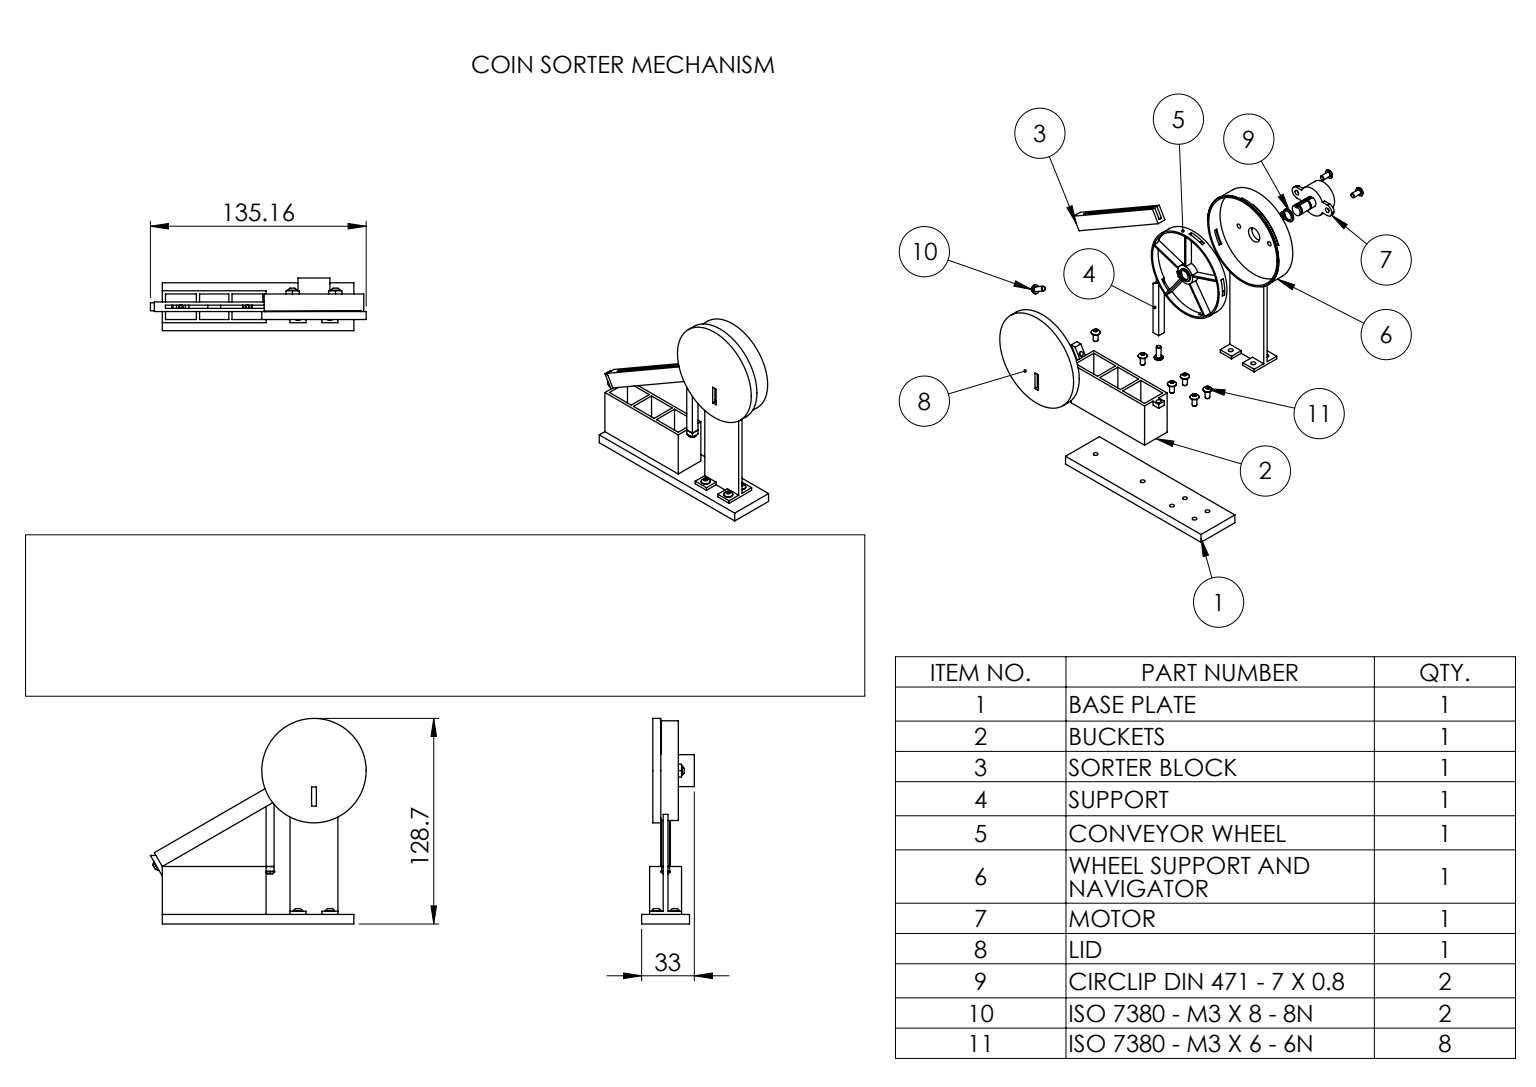
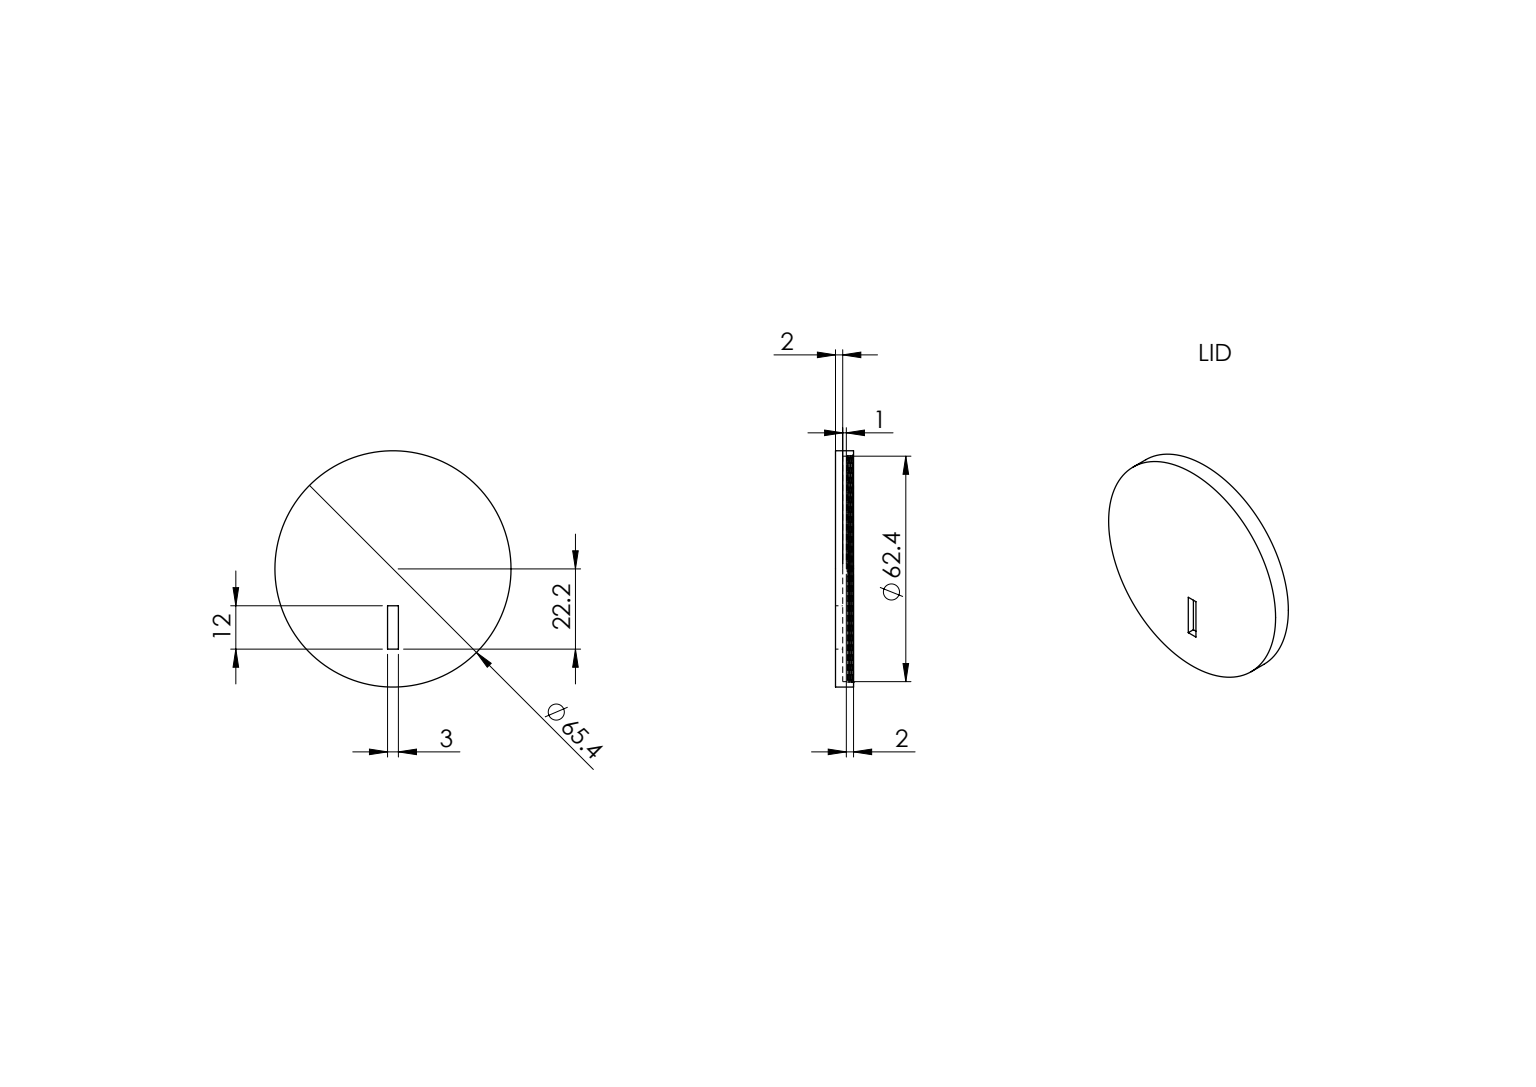
ISO-10303-21;
HEADER;
FILE_DESCRIPTION (('STEP AP214'),
    '1' );
FILE_NAME ('MAS-185',
    '2026-10-26T05:17:54',
    ( '' ),
    ( '' ),
    'SwSTEP 2.0',
    'SolidWorks 2026',
    '' );
FILE_SCHEMA (( 'AUTOMOTIVE_DESIGN' ));
ENDSEC;

DATA;
#1 = LINE ( 'NONE', #11989, #11081 ) ;
#2 = CARTESIAN_POINT ( 'NONE',  ( 35.00000000000000000, 126.3079067962035822, 4.690625000614518036 ) ) ;
#3 = ORIENTED_EDGE ( 'NONE', *, *, #1888, .T. ) ;
#4 = CARTESIAN_POINT ( 'NONE',  ( 35.00000000000000000, 126.3079067962035822, 4.296875000614517326 ) ) ;
#5 = AXIS2_PLACEMENT_3D ( 'NONE', #10923, #1108, #8837 ) ;
#6 = FACE_OUTER_BOUND ( 'NONE', #10030, .T. ) ;
#7 = ADVANCED_FACE ( 'NONE', ( #12422 ), #11435, .F. ) ;
#8 = DIRECTION ( 'NONE',  ( -0.000000000000000000, 1.000000000000000000, -0.000000000000000000 ) ) ;
#9 = CARTESIAN_POINT ( 'NONE',  ( 15.77218708916995560, 135.9950860171967975, 1.000000000000003109 ) ) ;
#10 = VECTOR ( 'NONE', #6065, 1000.000000000000000 ) ;
#11 = CARTESIAN_POINT ( 'NONE',  ( -6.666666666666660745, 2.000000000000001332, 1.599999999999986766 ) ) ;
#12 = ADVANCED_FACE ( 'NONE', ( #2550 ), #5478, .T. ) ;
#13 = CARTESIAN_POINT ( 'NONE',  ( 19.89999999999999503, 90.00000000000000000, -8.000000000000000000 ) ) ;
#14 = CARTESIAN_POINT ( 'NONE',  ( 20.00000000000000355, 121.2009999999999934, -1.499999999999999556 ) ) ;
#15 = ORIENTED_EDGE ( 'NONE', *, *, #11202, .T. ) ;
#16 = EDGE_CURVE ( 'NONE', #1898, #4275, #11568, .T. ) ;
#17 = CARTESIAN_POINT ( 'NONE',  ( 7.500000000000000000, 34.99999999999999289, -1.499999999999999556 ) ) ;
#18 = ORIENTED_EDGE ( 'NONE', *, *, #2781, .T. ) ;
#19 = EDGE_CURVE ( 'NONE', #6404, #5937, #10592, .T. ) ;
#20 = SURFACE_STYLE_FILL_AREA ( #10773 ) ;
#21 = CIRCLE ( 'NONE', #6519, 3.500000000000003109 ) ;
#22 = B_SPLINE_CURVE_WITH_KNOTS ( 'NONE', 3,
 ( #4736, #8602, #10562, #11406 ),
 .UNSPECIFIED., .F., .F.,
 ( 4, 4 ),
 ( 0.000000000000000000, 0.5999999999999992006 ),
 .UNSPECIFIED. ) ;
#23 = CARTESIAN_POINT ( 'NONE',  ( 65.00000000000000000, 90.00000000000000000, -3.000000000000000000 ) ) ;
#24 = LINE ( 'NONE', #4041, #9468 ) ;
#25 = PLANE ( 'NONE',  #12625 ) ;
#26 = ORIENTED_EDGE ( 'NONE', *, *, #8182, .F. ) ;
#27 = CARTESIAN_POINT ( 'NONE',  ( 33.50000000000000711, 79.80000000000001137, 8.000000000000000000 ) ) ;
#28 = CARTESIAN_POINT ( 'NONE',  ( 46.99999999999995737, 90.00000000000000000, -8.000000000000000000 ) ) ;
#29 = VERTEX_POINT ( 'NONE', #4640 ) ;
#30 = VECTOR ( 'NONE', #11564, 1000.000000000000114 ) ;
#31 =( NAMED_UNIT ( * ) SI_UNIT ( $, .STERADIAN. ) SOLID_ANGLE_UNIT ( ) );
#32 = CARTESIAN_POINT ( 'NONE',  ( 45.00000000000000000, 0.000000000000000000, -4.249999999999998224 ) ) ;
#33 = EDGE_LOOP ( 'NONE', ( #5496, #9068, #8693 ) ) ;
#34 = EDGE_CURVE ( 'NONE', #7938, #5032, #4885, .T. ) ;
#35 = DIRECTION ( 'NONE',  ( -0.000000000000000000, -0.000000000000000000, -1.000000000000000000 ) ) ;
#36 = VERTEX_POINT ( 'NONE', #3665 ) ;
#37 = LINE ( 'NONE', #7913, #8415 ) ;
#38 = CARTESIAN_POINT ( 'NONE',  ( 0.000000000000000000, -0.5773502691896255090, 1.000000000000000000 ) ) ;
#39 = VERTEX_POINT ( 'NONE', #7644 ) ;
#40 = COLOUR_RGB ( '',0.8941176470588234615, 0.8941176470588234615, 0.8941176470588234615 ) ;
#41 = VERTEX_POINT ( 'NONE', #12875 ) ;
#42 = FACE_BOUND ( 'NONE', #647, .T. ) ;
#43 = ORIENTED_EDGE ( 'NONE', *, *, #1360, .T. ) ;
#44 = CARTESIAN_POINT ( 'NONE',  ( 50.72178482187501203, 62.76906990284730625, 4.503125000614517148 ) ) ;
#45 = ORIENTED_EDGE ( 'NONE', *, *, #2569, .T. ) ;
#46 = DIRECTION ( 'NONE',  ( 0.000000000000000000, -0.000000000000000000, -1.000000000000000000 ) ) ;
#47 = ORIENTED_EDGE ( 'NONE', *, *, #5628, .T. ) ;
#48 = EDGE_CURVE ( 'NONE', #8414, #6329, #6123, .T. ) ;
#49 = VECTOR ( 'NONE', #8746, 1000.000000000000000 ) ;
#50 = DIRECTION ( 'NONE',  ( 0.000000000000000000, 0.000000000000000000, -1.000000000000000000 ) ) ;
#51 = CARTESIAN_POINT ( 'NONE',  ( 19.27821517812500574, 117.2309300971526937, 4.728125000614516793 ) ) ;
#52 = CARTESIAN_POINT ( 'NONE',  ( 50.59999999999999432, 117.0199925980744666, 4.850000000000000533 ) ) ;
#53 = FACE_OUTER_BOUND ( 'NONE', #7053, .T. ) ;
#54 = AXIS2_PLACEMENT_3D ( 'NONE', #9236, #4147, #9107 ) ;
#55 = APPLICATION_CONTEXT ( 'automotive_design' ) ;
#56 = PLANE ( 'NONE',  #9383 ) ;
#57 = EDGE_CURVE ( 'NONE', #11292, #8351, #9858, .T. ) ;
#59 = EDGE_CURVE ( 'NONE', #10107, #9996, #12197, .T. ) ;
#58 = VERTEX_POINT ( 'NONE', #1081 ) ;
#60 =( GEOMETRIC_REPRESENTATION_CONTEXT ( 3 ) GLOBAL_UNCERTAINTY_ASSIGNED_CONTEXT ( ( #12059 ) ) GLOBAL_UNIT_ASSIGNED_CONTEXT ( ( #6222, #10212, #383 ) ) REPRESENTATION_CONTEXT ( 'NONE', 'WORKASPACE' ) );
#61 =( BOUNDED_CURVE ( )  B_SPLINE_CURVE ( 2, ( #6392, #1163, #3141, #10390, #7315, #302, #10192 ),
 .UNSPECIFIED., .F., .F. ) 
 B_SPLINE_CURVE_WITH_KNOTS ( ( 3, 2, 2, 3 ),
 ( 0.000000000000000000, 0.03333333333333339532, 0.06666666666666679064, 0.1000000000000001860 ),
 .UNSPECIFIED. ) 
 CURVE ( )  GEOMETRIC_REPRESENTATION_ITEM ( )  RATIONAL_B_SPLINE_CURVE ( ( 1.000000000000000000, 0.8660254037844387076, 1.000000000000000000, 0.8660254037844387076, 1.000000000000000000, 0.8660254037844380415, 1.000000000000000666 ) ) 
 REPRESENTATION_ITEM ( '' )  );
#62 = CARTESIAN_POINT ( 'NONE',  ( 50.60000000000001563, 62.98000740192552627, 4.700000000000000178 ) ) ;
#63 = DIRECTION ( 'NONE',  ( 0.000000000000000000, 0.000000000000000000, 1.000000000000000000 ) ) ;
#64 = CARTESIAN_POINT ( 'NONE',  ( 42.76092309580126027, 120.3492821251987550, 2.999999999999998668 ) ) ;
#65 = ORIENTED_EDGE ( 'NONE', *, *, #9345, .T. ) ;
#66 = AXIS2_PLACEMENT_3D ( 'NONE', #9653, #8676, #680 ) ;
#67 = DIRECTION ( 'NONE',  ( 0.000000000000000000, 1.000000000000000000, 0.000000000000000000 ) ) ;
#68 = ORIENTED_EDGE ( 'NONE', *, *, #7335, .T. ) ;
#69 = CARTESIAN_POINT ( 'NONE',  ( 17.26299177799148055, 43.12143982588584379, 1.000000000000003109 ) ) ;
#70 = LINE ( 'NONE', #8139, #12259 ) ;
#71 = ORIENTED_EDGE ( 'NONE', *, *, #3443, .T. ) ;
#72 = CARTESIAN_POINT ( 'NONE',  ( -1.000000000000000000, -4.873461295629625489, -0.8000000000000000444 ) ) ;
#73 = CARTESIAN_POINT ( 'NONE',  ( 66.44356964374999563, 71.84604660189820891, 4.146875000614517859 ) ) ;
#74 = DIRECTION ( 'NONE',  ( 0.000000000000000000, 0.000000000000000000, 1.000000000000000000 ) ) ;
#75 = FACE_BOUND ( 'NONE', #11702, .T. ) ;
#76 = AXIS2_PLACEMENT_3D ( 'NONE', #9120, #143, #2199 ) ;
#77 = VECTOR ( 'NONE', #7626, 1000.000000000000000 ) ;
#78 = PLANE ( 'NONE',  #12219 ) ;
#79 = CARTESIAN_POINT ( 'NONE',  ( 9.999999999999994671, 27.00000000000000000, -2.500000000000000000 ) ) ;
#80 = FACE_BOUND ( 'NONE', #12190, .T. ) ;
#81 = EDGE_CURVE ( 'NONE', #9930, #10652, #10526, .T. ) ;
#82 = FACE_OUTER_BOUND ( 'NONE', #972, .T. ) ;
#83 = AXIS2_PLACEMENT_3D ( 'NONE', #3379, #1527, #7355 ) ;
#84 = DIRECTION ( 'NONE',  ( 2.891205793294679312E-17, 0.000000000000000000, -1.000000000000000000 ) ) ;
#85 = VERTEX_POINT ( 'NONE', #9987 ) ;
#86 = VECTOR ( 'NONE', #8647, 1000.000000000000000 ) ;
#87 = PLANE ( 'NONE',  #9136 ) ;
#88 = ORIENTED_EDGE ( 'NONE', *, *, #8982, .F. ) ;
#89 = CARTESIAN_POINT ( 'NONE',  ( -63.73205080756886076, 30.46410161513775350, 0.000000000000000000 ) ) ;
#90 = CARTESIAN_POINT ( 'NONE',  ( 3.800000000000001155, 108.0133283987163111, 4.175000001229035362 ) ) ;
#91 = AXIS2_PLACEMENT_3D ( 'NONE', #12672, #7630, #11620 ) ;
#92 = PRODUCT_DEFINITION_SHAPE ( 'NONE', 'NONE',  #12958 ) ;
#93 = DIRECTION ( 'NONE',  ( -1.000000000000000000, 0.000000000000000000, -5.337610695313252124E-17 ) ) ;
#94 = CIRCLE ( 'NONE', #5951, 0.9999999999999991118 ) ;
#95 = ORIENTED_EDGE ( 'NONE', *, *, #10637, .F. ) ;
#96 = FACE_OUTER_BOUND ( 'NONE', #3585, .T. ) ;
#97 = EDGE_CURVE ( 'NONE', #1488, #5076, #12936, .T. ) ;
#98 = CARTESIAN_POINT ( 'NONE',  ( 66.19999999999993179, 71.98667160128364628, 3.837499999999999911 ) ) ;
#99 = ORIENTED_EDGE ( 'NONE', *, *, #9615, .F. ) ;
#100 = SURFACE_SIDE_STYLE ('',( #3136 ) ) ;
#101 = CYLINDRICAL_SURFACE ( 'NONE', #2852, 1.500000000000002665 ) ;
#102 = ORIENTED_EDGE ( 'NONE', *, *, #8081, .F. ) ;
#104 = ORIENTED_EDGE ( 'NONE', *, *, #6904, .F. ) ;
#103 = CIRCLE ( 'NONE', #2000, 3.500000000000003109 ) ;
#105 = AXIS2_PLACEMENT_3D ( 'NONE', #1700, #5689, #8636 ) ;
#106 = DIRECTION ( 'NONE',  ( 0.000000000000000000, 0.000000000000000000, 1.000000000000000000 ) ) ;
#107 = DIRECTION ( 'NONE',  ( -1.000000000000000000, 0.000000000000000000, 0.000000000000000000 ) ) ;
#108 = VERTEX_POINT ( 'NONE', #7965 ) ;
#109 = EDGE_CURVE ( 'NONE', #7067, #112, #11947, .T. ) ;
#110 = ORIENTED_EDGE ( 'NONE', *, *, #11359, .T. ) ;
#111 = FACE_OUTER_BOUND ( 'NONE', #2814, .T. ) ;
#112 = VERTEX_POINT ( 'NONE', #12017 ) ;
#113 = APPLICATION_PROTOCOL_DEFINITION ( 'draft international standard', 'automotive_design', 1998, #3183 ) ;
#114 = CARTESIAN_POINT ( 'NONE',  ( 66.44356964374999563, 71.84604660189820891, 4.090625000614517504 ) ) ;
#115 = VECTOR ( 'NONE', #5469, 1000.000000000000000 ) ;
#116 = ORIENTED_EDGE ( 'NONE', *, *, #12848, .F. ) ;
#117 = CARTESIAN_POINT ( 'NONE',  ( -43.33333333333332860, 79.07477288111861924, -1.000000000000001110 ) ) ;
#118 = EDGE_LOOP ( 'NONE', ( #5135, #6023 ) ) ;
#119 = DIRECTION ( 'NONE',  ( 0.000000000000000000, 0.5000000000000000000, -0.8660254037844385966 ) ) ;
#120 = CARTESIAN_POINT ( 'NONE',  ( 19.27821517812503060, 62.76906990284727783, 3.078125000614517326 ) ) ;
#121 = DIRECTION ( 'NONE',  ( -0.8665440819333538602, -0.4991005450470686888, -4.805464830191153728E-17 ) ) ;
#122 = CARTESIAN_POINT ( 'NONE',  ( 35.00000000000000711, 53.97334320256736362, 3.425000001229034474 ) ) ;
#123 = AXIS2_PLACEMENT_3D ( 'NONE', #3186, #84, #7099 ) ;
#124 = CARTESIAN_POINT ( 'NONE',  ( 50.60000000000001563, 62.98000740192552627, 4.250000000000000000 ) ) ;
#125 = ADVANCED_FACE ( 'NONE', ( #2807 ), #25, .T. ) ;
#126 = ORIENTED_EDGE ( 'NONE', *, *, #19, .T. ) ;
#127 = CARTESIAN_POINT ( 'NONE',  ( 3.800000000000025135, 71.98667160128366049, 4.587500000000001243 ) ) ;
#128 = DIRECTION ( 'NONE',  ( 0.000000000000000000, 0.000000000000000000, -1.000000000000000000 ) ) ;
#129 = CARTESIAN_POINT ( 'NONE',  ( 59.24587011312613072, 109.7457631344924778, 2.999999999999999556 ) ) ;
#130 = ORIENTED_EDGE ( 'NONE', *, *, #2719, .F. ) ;
#131 = CARTESIAN_POINT ( 'NONE',  ( 1.040000000000000036, 0.5773502691896263972, -1.000000000000000000 ) ) ;
#132 = ORIENTED_EDGE ( 'NONE', *, *, #9753, .F. ) ;
#133 = LINE ( 'NONE', #6034, #1273 ) ;
#134 = CARTESIAN_POINT ( 'NONE',  ( 35.00000000000000000, 126.3079067962035822, 2.890625000614516882 ) ) ;
#135 = ORIENTED_EDGE ( 'NONE', *, *, #4811, .F. ) ;
#136 = EDGE_CURVE ( 'NONE', #12578, #3097, #7900, .T. ) ;
#137 = CARTESIAN_POINT ( 'NONE',  ( 66.44356964374998142, 108.1539533981018053, 3.321875000614517237 ) ) ;
#138 = DIRECTION ( 'NONE',  ( 0.000000000000000000, 0.000000000000000000, 1.000000000000000000 ) ) ;
#139 = DIRECTION ( 'NONE',  ( 0.000000000000000000, -0.000000000000000000, -1.000000000000000000 ) ) ;
#140 = CARTESIAN_POINT ( 'NONE',  ( -1.000000000000000000, -5.473461295629626022, -0.8000000000000000444 ) ) ;
#141 = ADVANCED_FACE ( 'NONE', ( #3852 ), #10839, .F. ) ;
#142 = DIRECTION ( 'NONE',  ( -0.000000000000000000, 0.000000000000000000, -1.000000000000000000 ) ) ;
#143 = DIRECTION ( 'NONE',  ( 0.8660254037844394848, 0.4999999999999985012, -0.000000000000000000 ) ) ;
#144 = DIRECTION ( 'NONE',  ( 0.000000000000000000, 0.000000000000000000, 1.000000000000000000 ) ) ;
#145 = CARTESIAN_POINT ( 'NONE',  ( 34.25000000000000000, 92.49999999999998579, 4.800000000000000711 ) ) ;
#146 = DIRECTION ( 'NONE',  ( 1.000000000000000000, 0.000000000000000000, 0.000000000000000000 ) ) ;
#147 = ORIENTED_EDGE ( 'NONE', *, *, #622, .F. ) ;
#148 = VECTOR ( 'NONE', #2125, 1000.000000000000000 ) ;
#149 = EDGE_CURVE ( 'NONE', #10256, #6226, #4830, .T. ) ;
#150 = FACE_OUTER_BOUND ( 'NONE', #10972, .T. ) ;
#151 = ORIENTED_EDGE ( 'NONE', *, *, #731, .F. ) ;
#152 =( NAMED_UNIT ( * ) SI_UNIT ( $, .STERADIAN. ) SOLID_ANGLE_UNIT ( ) );
#153 = DIRECTION ( 'NONE',  ( 1.000000000000000000, 0.000000000000000000, 0.000000000000000000 ) ) ;
#154 = CARTESIAN_POINT ( 'NONE',  ( -16.33333333333332504, 2.000000000000000000, -7.999999999999996447 ) ) ;
#155 = DIRECTION ( 'NONE',  ( -1.000000000000000000, 0.000000000000000000, -0.000000000000000000 ) ) ;
#156 = VECTOR ( 'NONE', #8810, 1000.000000000000000 ) ;
#157 = ORIENTED_EDGE ( 'NONE', *, *, #725, .T. ) ;
#158 = CARTESIAN_POINT ( 'NONE',  ( 50.00000000000000000, 2.000000000000001776, 1.500000000000001332 ) ) ;
#159 = LINE ( 'NONE', #2018, #4188 ) ;
#160 = ORIENTED_EDGE ( 'NONE', *, *, #4406, .F. ) ;
#161 = FILL_AREA_STYLE_COLOUR ( '', #4733 ) ;
#162 = ORIENTED_EDGE ( 'NONE', *, *, #11234, .F. ) ;
#163 =( LENGTH_UNIT ( ) NAMED_UNIT ( * ) SI_UNIT ( .MILLI., .METRE. ) );
#164 = ORIENTED_EDGE ( 'NONE', *, *, #8938, .T. ) ;
#165 = AXIS2_PLACEMENT_3D ( 'NONE', #5058, #1689, #12557 ) ;
#166 = LINE ( 'NONE', #6266, #6322 ) ;
#167 = CYLINDRICAL_SURFACE ( 'NONE', #2062, 31.19999999999999929 ) ;
#168 = EDGE_CURVE ( 'NONE', #9993, #9602, #10963, .T. ) ;
#169 = VERTEX_POINT ( 'NONE', #6912 ) ;
#170 = PRODUCT_DEFINITION_CONTEXT ( 'detailed design', #1838, 'design' ) ;
#171 = ORIENTED_EDGE ( 'NONE', *, *, #11272, .F. ) ;
#173 = DIRECTION ( 'NONE',  ( -0.000000000000000000, -0.000000000000000000, -1.000000000000000000 ) ) ;
#172 = AXIS2_PLACEMENT_3D ( 'NONE', #7936, #11922, #10932 ) ;
#174 = EDGE_LOOP ( 'NONE', ( #6858, #8002, #3578, #927 ) ) ;
#175 = APPLICATION_PROTOCOL_DEFINITION ( 'draft international standard', 'automotive_design', 1998, #11522 ) ;
#176 = CARTESIAN_POINT ( 'NONE',  ( 50.72178482187499071, 117.2309300971526937, 3.753125000614517592 ) ) ;
#177 = AXIS2_PLACEMENT_3D ( 'NONE', #10077, #4014, #1048 ) ;
#178 = ORIENTED_EDGE ( 'NONE', *, *, #6430, .T. ) ;
#179 = DIRECTION ( 'NONE',  ( 0.000000000000000000, 0.000000000000000000, 1.000000000000000000 ) ) ;
#180 = CARTESIAN_POINT ( 'NONE',  ( -56.80384757729341771, 34.46410161513777837, 0.000000000000000000 ) ) ;
#181 = ORIENTED_EDGE ( 'NONE', *, *, #7547, .F. ) ;
#182 = CARTESIAN_POINT ( 'NONE',  ( -60.38397459621558738, 30.66506350946110260, 0.000000000000000000 ) ) ;
#183 = CARTESIAN_POINT ( 'NONE',  ( 50.72178482187499071, 117.2309300971526937, 4.203125000614517326 ) ) ;
#184 = EDGE_CURVE ( 'NONE', #4807, #7972, #8814, .T. ) ;
#185 = DIRECTION ( 'NONE',  ( -0.3553942263724512163, 0.9347165045408831752, 0.000000000000000000 ) ) ;
#186 = AXIS2_PLACEMENT_3D ( 'NONE', #1840, #9816, #9754 ) ;
#187 = DIRECTION ( 'NONE',  ( -0.000000000000000000, -0.000000000000000000, -1.000000000000000000 ) ) ;
#188 = EDGE_CURVE ( 'NONE', #5860, #7119, #2800, .T. ) ;
#189 = ORIENTED_EDGE ( 'NONE', *, *, #6067, .T. ) ;
#190 = CARTESIAN_POINT ( 'NONE',  ( 19.40000000000000924, 117.0199925980744666, 3.125000000000000000 ) ) ;
#191 = VERTEX_POINT ( 'NONE', #1882 ) ;
#192 = LINE ( 'NONE', #5111, #8966 ) ;
#193 = VERTEX_POINT ( 'NONE', #2014 ) ;
#194 = CIRCLE ( 'NONE', #6260, 3.499999999999996003 ) ;
#195 = FACE_OUTER_BOUND ( 'NONE', #1919, .T. ) ;
#196 = ORIENTED_EDGE ( 'NONE', *, *, #12600, .T. ) ;
#197 = DIRECTION ( 'NONE',  ( -0.000000000000000000, -1.000000000000000000, -0.000000000000000000 ) ) ;
#198 = CARTESIAN_POINT ( 'NONE',  ( 3.556430356250028790, 71.84604660189818048, 3.940625000614518036 ) ) ;
#199 = EDGE_LOOP ( 'NONE', ( #6657, #5220, #2552, #8518 ) ) ;
#200 = EDGE_CURVE ( 'NONE', #11286, #1104, #9001, .T. ) ;
#201 = CARTESIAN_POINT ( 'NONE',  ( 35.00000000000000711, 53.69209320379640360, 4.071875000614516793 ) ) ;
#202 = DIRECTION ( 'NONE',  ( -0.5000000000000042188, 0.8660254037844362651, 0.000000000000000000 ) ) ;
#203 = PRODUCT_DEFINITION_SHAPE ( 'NONE', 'NONE',  #12962 ) ;
#204 = LINE ( 'NONE', #1265, #6022 ) ;
#205 = AXIS2_PLACEMENT_3D ( 'NONE', #12610, #4630, #6775 ) ;
#206 = CARTESIAN_POINT ( 'NONE',  ( 66.19999999999988916, 71.98667160128361786, 3.950000001229034829 ) ) ;
#207 = DIRECTION ( 'NONE',  ( -1.000000000000000000, 0.000000000000000000, 0.000000000000000000 ) ) ;
#208 = DIRECTION ( 'NONE',  ( -0.8660254037844365982, -0.5000000000000036637, 0.000000000000000000 ) ) ;
#209 = DIRECTION ( 'NONE',  ( 0.000000000000000000, 0.000000000000000000, 1.000000000000000000 ) ) ;
#210 = VECTOR ( 'NONE', #6420, 1000.000000000000000 ) ;
#211 = CARTESIAN_POINT ( 'NONE',  ( 1.040000000000000036, -1.154700538379251240, 1.014316938424154191E-17 ) ) ;
#212 = CARTESIAN_POINT ( 'NONE',  ( -48.33333333333332860, -5.000000000000000000, -1.500000000000003109 ) ) ;
#213 = ORIENTED_EDGE ( 'NONE', *, *, #1279, .T. ) ;
#214 = EDGE_CURVE ( 'NONE', #1472, #1154, #10317, .T. ) ;
#215 = FACE_OUTER_BOUND ( 'NONE', #2493, .T. ) ;
#216 = VERTEX_POINT ( 'NONE', #11026 ) ;
#217 = FILL_AREA_STYLE ('',( #283 ) ) ;
#218 = AXIS2_PLACEMENT_3D ( 'NONE', #4134, #11252, #317 ) ;
#219 = DIRECTION ( 'NONE',  ( 0.000000000000000000, 0.000000000000000000, -1.000000000000000000 ) ) ;
#220 = LINE ( 'NONE', #6117, #2380 ) ;
#221 = ADVANCED_FACE ( 'NONE', ( #5806 ), #2080, .F. ) ;
#222 = PLANE ( 'NONE',  #9692 ) ;
#223 = ADVANCED_FACE ( 'NONE', ( #9797 ), #3264, .F. ) ;
#224 = ORIENTED_EDGE ( 'NONE', *, *, #6026, .F. ) ;
#225 = DIRECTION ( 'NONE',  ( -0.000000000000000000, 0.000000000000000000, -1.000000000000000000 ) ) ;
#226 = DIRECTION ( 'NONE',  ( -0.000000000000000000, 1.000000000000000000, -0.000000000000000000 ) ) ;
#227 = ORIENTED_EDGE ( 'NONE', *, *, #6357, .F. ) ;
#228 =( NAMED_UNIT ( * ) SI_UNIT ( $, .STERADIAN. ) SOLID_ANGLE_UNIT ( ) );
#229 = PLANE ( 'NONE',  #10368 ) ;
#230 = ORIENTED_EDGE ( 'NONE', *, *, #426, .T. ) ;
#231 = VECTOR ( 'NONE', #9140, 1000.000000000000000 ) ;
#232 = APPLICATION_CONTEXT ( 'automotive_design' ) ;
#233 = ORIENTED_EDGE ( 'NONE', *, *, #6025, .F. ) ;
#234 = CARTESIAN_POINT ( 'NONE',  ( 2.300000000000003375, 90.00000000000000000, 3.000000000000000000 ) ) ;
#235 = DIRECTION ( 'NONE',  ( -1.000000000000000000, 0.000000000000000000, 0.000000000000000000 ) ) ;
#236 = ORIENTED_EDGE ( 'NONE', *, *, #952, .F. ) ;
#237 = VERTEX_POINT ( 'NONE', #12343 ) ;
#238 = CIRCLE ( 'NONE', #3615, 3.499999999999996003 ) ;
#239 = DIRECTION ( 'NONE',  ( 0.000000000000000000, 0.000000000000000000, -1.000000000000000000 ) ) ;
#240 = ORIENTED_EDGE ( 'NONE', *, *, #10021, .T. ) ;
#241 = CARTESIAN_POINT ( 'NONE',  ( 50.72178482187501203, 62.76906990284730625, 3.603125000614517681 ) ) ;
#242 = VERTEX_POINT ( 'NONE', #9265 ) ;
#243 = CARTESIAN_POINT ( 'NONE',  ( 4.336808689942017736E-16, 0.000000000000000000, 0.000000000000000000 ) ) ;
#244 = EDGE_CURVE ( 'NONE', #12399, #6272, #479, .T. ) ;
#245 = DIRECTION ( 'NONE',  ( -1.000000000000000000, 0.000000000000000000, -0.000000000000000000 ) ) ;
#246 = ORIENTED_EDGE ( 'NONE', *, *, #10941, .F. ) ;
#247 = DIRECTION ( 'NONE',  ( 0.000000000000000000, 0.000000000000000000, 1.000000000000000000 ) ) ;
#248 = DIRECTION ( 'NONE',  ( 1.049727191973305517E-16, 0.5150380737757253025, -0.8571673013836857979 ) ) ;
#249 = VECTOR ( 'NONE', #11495, 1000.000000000000000 ) ;
#250 = CARTESIAN_POINT ( 'NONE',  ( 50.09999999999995168, 90.00000000000000000, -10.00000000000000000 ) ) ;
#251 = FACE_OUTER_BOUND ( 'NONE', #2972, .T. ) ;
#252 = VERTEX_POINT ( 'NONE', #288 ) ;
#253 = CARTESIAN_POINT ( 'NONE',  ( 35.00000000000000711, 53.97334320256736362, 3.762500000000000178 ) ) ;
#254 = EDGE_CURVE ( 'NONE', #5137, #10011, #5741, .T. ) ;
#255 = VERTEX_POINT ( 'NONE', #12080 ) ;
#256 = DIRECTION ( 'NONE',  ( 0.000000000000000000, 0.000000000000000000, 1.000000000000000000 ) ) ;
#257 = ORIENTED_EDGE ( 'NONE', *, *, #8326, .F. ) ;
#258 =( GEOMETRIC_REPRESENTATION_CONTEXT ( 3 ) GLOBAL_UNCERTAINTY_ASSIGNED_CONTEXT ( ( #6606 ) ) GLOBAL_UNIT_ASSIGNED_CONTEXT ( ( #8219, #3259, #10305 ) ) REPRESENTATION_CONTEXT ( 'NONE', 'WORKASPACE' ) );
#259 = CYLINDRICAL_SURFACE ( 'NONE', #10517, 31.19999999999998863 ) ;
#260 = ADVANCED_FACE ( 'NONE', ( #3129 ), #3324, .T. ) ;
#261 = VERTEX_POINT ( 'NONE', #1283 ) ;
#262 = FACE_OUTER_BOUND ( 'NONE', #6852, .T. ) ;
#263 = AXIS2_PLACEMENT_3D ( 'NONE', #117, #3851, #2872 ) ;
#264 = CARTESIAN_POINT ( 'NONE',  ( 19.27821517812500574, 117.2309300971526937, 4.728125000614516793 ) ) ;
#265 = CARTESIAN_POINT ( 'NONE',  ( 3.556430356250014579, 108.1539533981018053, 3.021875000614517415 ) ) ;
#266 = LINE ( 'NONE', #12261, #1845 ) ;
#267 = CARTESIAN_POINT ( 'NONE',  ( 31.59522469073171891, 84.46307801270442894, 22.38477631085024555 ) ) ;
#268 = STYLED_ITEM ( 'NONE', ( #1181 ), #2639 ) ;
#269 = FACE_OUTER_BOUND ( 'NONE', #11895, .T. ) ;
#270 = AXIS2_PLACEMENT_3D ( 'NONE', #2486, #11695, #10523 ) ;
#271 = EDGE_CURVE ( 'NONE', #3833, #3097, #6317, .T. ) ;
#272 = CARTESIAN_POINT ( 'NONE',  ( 12.66025403784434822, 85.80682368868758658, 1.000000000000000000 ) ) ;
#273 = CARTESIAN_POINT ( 'NONE',  ( -60.00000000000000000, 23.99999999999998934, 2.500000000000000000 ) ) ;
#274 = CARTESIAN_POINT ( 'NONE',  ( 44.20597631976078645, 117.5000000000000568, 4.000000000000000000 ) ) ;
#275 = AXIS2_PLACEMENT_3D ( 'NONE', #3462, #8298, #7442 ) ;
#276 = DIRECTION ( 'NONE',  ( 1.000000000000000000, 0.000000000000000000, 0.000000000000000000 ) ) ;
#277 = CARTESIAN_POINT ( 'NONE',  ( 3.556430356250014579, 108.1539533981018053, 3.471875000614516704 ) ) ;
#278 = ORIENTED_EDGE ( 'NONE', *, *, #5223, .F. ) ;
#279 = DIRECTION ( 'NONE',  ( -0.5877852522924753575, 0.8090169943749458970, 0.000000000000000000 ) ) ;
#280 = ORIENTED_EDGE ( 'NONE', *, *, #1510, .F. ) ;
#281 = CIRCLE ( 'NONE', #7814, 4.338286831716297698 ) ;
#282 = PRODUCT ( 'lid', 'lid', '', ( #4128 ) ) ;
#283 = FILL_AREA_STYLE_COLOUR ( '', #7592 ) ;
#284 = AXIS2_PLACEMENT_3D ( 'NONE', #3967, #808, #3834 ) ;
#285 = DIRECTION ( 'NONE',  ( 0.000000000000000000, 0.000000000000000000, -1.000000000000000000 ) ) ;
#286 = FACE_OUTER_BOUND ( 'NONE', #5183, .T. ) ;
#287 = ADVANCED_FACE ( 'NONE', ( #7172 ), #1536, .F. ) ;
#288 = CARTESIAN_POINT ( 'NONE',  ( 50.09999999999995168, 90.00000000000000000, -8.000000000000000000 ) ) ;
#289 = EDGE_LOOP ( 'NONE', ( #1284, #1485, #7281, #1532 ) ) ;
#290 = AXIS2_PLACEMENT_3D ( 'NONE', #12563, #2683, #9478 ) ;
#291 = CARTESIAN_POINT ( 'NONE',  ( 35.75000000000000711, 92.49999999999998579, 4.000000000000000000 ) ) ;
#292 = CARTESIAN_POINT ( 'NONE',  ( 35.00000000000000000, 90.00000000000000000, 4.000000000000000000 ) ) ;
#293 = VECTOR ( 'NONE', #10096, 1000.000000000000000 ) ;
#294 = VERTEX_POINT ( 'NONE', #6118 ) ;
#295 =( BOUNDED_CURVE ( )  B_SPLINE_CURVE ( 2, ( #8455, #11652, #1581, #11588, #2506, #12579, #9564 ),
 .UNSPECIFIED., .F., .F. ) 
 B_SPLINE_CURVE_WITH_KNOTS ( ( 3, 2, 2, 3 ),
 ( 0.5999999999999999778, 0.6333333333333334147, 0.6666666666666667407, 0.7000000000000001776 ),
 .UNSPECIFIED. ) 
 CURVE ( )  GEOMETRIC_REPRESENTATION_ITEM ( )  RATIONAL_B_SPLINE_CURVE ( ( 1.000000000000000000, 0.8660254037844387076, 1.000000000000000000, 0.8660254037844387076, 1.000000000000000000, 0.8660254037844378194, 1.000000000000000888 ) ) 
 REPRESENTATION_ITEM ( '' )  );
#296 = CARTESIAN_POINT ( 'NONE',  ( 35.00000000000000000, 90.00000000000000000, -3.000000000000000000 ) ) ;
#297 = CARTESIAN_POINT ( 'NONE',  ( 52.49999999999996447, 94.00000000000000000, -10.00000000000000000 ) ) ;
#298 = ORIENTED_EDGE ( 'NONE', *, *, #5640, .T. ) ;
#299 = ORIENTED_EDGE ( 'NONE', *, *, #12486, .F. ) ;
#300 = EDGE_CURVE ( 'NONE', #9165, #9156, #9132, .T. ) ;
#301 = EDGE_CURVE ( 'NONE', #5352, #12120, #2388, .T. ) ;
#302 = CARTESIAN_POINT ( 'NONE',  ( 66.20000000000005969, 108.0133283987162685, 4.475000001229034297 ) ) ;
#303 = DIRECTION ( 'NONE',  ( -1.000000000000000000, 0.000000000000000000, 4.336808689942017243E-16 ) ) ;
#304 = VECTOR ( 'NONE', #4833, 1000.000000000000000 ) ;
#305 = ORIENTED_EDGE ( 'NONE', *, *, #8048, .F. ) ;
#306 = VECTOR ( 'NONE', #308, 1000.000000000000114 ) ;
#307 = VERTEX_POINT ( 'NONE', #5210 ) ;
#308 = DIRECTION ( 'NONE',  ( 0.8660254037844361541, 0.5000000000000042188, 0.000000000000000000 ) ) ;
#309 = VERTEX_POINT ( 'NONE', #6189 ) ;
#310 = EDGE_CURVE ( 'NONE', #8511, #12562, #11290, .T. ) ;
#311 = CARTESIAN_POINT ( 'NONE',  ( 50.72178482187501203, 62.76906990284730625, 4.053125000614517859 ) ) ;
#312 = ORIENTED_EDGE ( 'NONE', *, *, #4163, .F. ) ;
#313 = CIRCLE ( 'NONE', #9312, 30.19999999999999218 ) ;
#314 = LINE ( 'NONE', #2362, #12520 ) ;
#315 = ORIENTED_EDGE ( 'NONE', *, *, #7224, .T. ) ;
#316 = VECTOR ( 'NONE', #11418, 1000.000000000000000 ) ;
#317 = DIRECTION ( 'NONE',  ( 1.000000000000000000, 0.000000000000000000, 0.000000000000000000 ) ) ;
#318 = DIRECTION ( 'NONE',  ( 0.000000000000000000, 0.000000000000000000, 1.000000000000000000 ) ) ;
#319 = LINE ( 'NONE', #8516, #3101 ) ;
#320 = CONICAL_SURFACE ( 'NONE', #5556, 1732.050807568857181, 1.047197551196592746 ) ;
#321 = DIRECTION ( 'NONE',  ( -0.000000000000000000, -0.000000000000000000, -1.000000000000000000 ) ) ;
#322 = EDGE_CURVE ( 'NONE', #7840, #11587, #9067, .T. ) ;
#323 = ORIENTED_EDGE ( 'NONE', *, *, #9643, .F. ) ;
#324 =( GEOMETRIC_REPRESENTATION_CONTEXT ( 3 ) GLOBAL_UNCERTAINTY_ASSIGNED_CONTEXT ( ( #7109 ) ) GLOBAL_UNIT_ASSIGNED_CONTEXT ( ( #5148, #12551, #626 ) ) REPRESENTATION_CONTEXT ( 'NONE', 'WORKASPACE' ) );
#325 = CARTESIAN_POINT ( 'NONE',  ( 3.556430356250015024, 90.00000000000000000, 4.859375000614517326 ) ) ;
#326 = ORIENTED_EDGE ( 'NONE', *, *, #12262, .F. ) ;
#327 = CARTESIAN_POINT ( 'NONE',  ( 5.011331584521381721, 81.39071625125095011, -1.000000000000000000 ) ) ;
#328 = ORIENTED_EDGE ( 'NONE', *, *, #4950, .F. ) ;
#329 = DIRECTION ( 'NONE',  ( -0.8660254037844360431, -0.5000000000000045519, 0.000000000000000000 ) ) ;
#330 = VERTEX_POINT ( 'NONE', #11158 ) ;
#331 = LINE ( 'NONE', #11396, #210 ) ;
#332 = CARTESIAN_POINT ( 'NONE',  ( 8.335915615093540509, 106.7866562222949938, 3.000000000000001776 ) ) ;
#333 = CIRCLE ( 'NONE', #7661, 2.849999999999999201 ) ;
#334 = CARTESIAN_POINT ( 'NONE',  ( 50.72178482187499071, 117.2309300971526937, 2.909375000614517148 ) ) ;
#335 = ADVANCED_FACE ( 'NONE', ( #1345 ), #222, .F. ) ;
#336 = DIRECTION ( 'NONE',  ( 0.000000000000000000, 0.000000000000000000, 1.000000000000000000 ) ) ;
#337 = DIRECTION ( 'NONE',  ( -0.000000000000000000, -0.000000000000000000, -1.000000000000000000 ) ) ;
#338 = ADVANCED_FACE ( 'NONE', ( #7108, #5337 ), #2214, .T. ) ;
#339 = DIRECTION ( 'NONE',  ( -0.5877852522924715828, -0.8090169943749484505, 0.000000000000000000 ) ) ;
#340 = CARTESIAN_POINT ( 'NONE',  ( 66.19999999999998863, 90.00000000000000000, 4.325000000000000178 ) ) ;
#341 = DIRECTION ( 'NONE',  ( -0.3262398754384822630, 0.9452870165584014162, 0.000000000000000000 ) ) ;
#342 = VECTOR ( 'NONE', #6084, 1000.000000000000000 ) ;
#343 = LINE ( 'NONE', #3380, #2212 ) ;
#344 = CARTESIAN_POINT ( 'NONE',  ( 41.31805916882746743, 91.52713075379783447, 22.38477631085024555 ) ) ;
#345 = CARTESIAN_POINT ( 'NONE',  ( 35.00000000000000711, 53.69209320379639649, 3.621875000614517059 ) ) ;
#346 = ORIENTED_EDGE ( 'NONE', *, *, #1264, .T. ) ;
#347 = DIRECTION ( 'NONE',  ( -0.000000000000000000, 1.000000000000000000, -0.000000000000000000 ) ) ;
#348 = ORIENTED_EDGE ( 'NONE', *, *, #6229, .T. ) ;
#349 = EDGE_CURVE ( 'NONE', #2081, #11940, #2919, .T. ) ;
#350 = AXIS2_PLACEMENT_3D ( 'NONE', #7687, #12398, #1471 ) ;
#351 = ADVANCED_FACE ( 'NONE', ( #11353 ), #2405, .T. ) ;
#352 = DIRECTION ( 'NONE',  ( -1.000000000000000000, 0.000000000000000000, 0.000000000000000000 ) ) ;
#353 = CARTESIAN_POINT ( 'NONE',  ( 62.42613047537196991, 99.43702109502110886, 4.000000000000000000 ) ) ;
#354 = CARTESIAN_POINT ( 'NONE',  ( 17.55170909815984004, 66.83416404266884570, 4.000000000000000000 ) ) ;
#355 = ORIENTED_EDGE ( 'NONE', *, *, #8194, .T. ) ;
#356 = DIRECTION ( 'NONE',  ( -1.000000000000000000, 0.000000000000000000, 0.000000000000000000 ) ) ;
#357 = DIRECTION ( 'NONE',  ( -1.000000000000000000, -0.000000000000000000, -0.000000000000000000 ) ) ;
#358 = AXIS2_PLACEMENT_3D ( 'NONE', #3613, #12439, #9423 ) ;
#359 = ORIENTED_EDGE ( 'NONE', *, *, #812, .T. ) ;
#360 = DIRECTION ( 'NONE',  ( 1.000000000000000000, 0.000000000000000000, 0.000000000000000000 ) ) ;
#361 = CARTESIAN_POINT ( 'NONE',  ( 35.00000000000000000, 90.00000000000000000, -1.499999999999999556 ) ) ;
#362 = VERTEX_POINT ( 'NONE', #4108 ) ;
#363 = ORIENTED_EDGE ( 'NONE', *, *, #11341, .T. ) ;
#364 = EDGE_CURVE ( 'NONE', #1906, #5411, #4011, .T. ) ;
#365 = LINE ( 'NONE', #2416, #4028 ) ;
#366 = LINE ( 'NONE', #8567, #6016 ) ;
#367 = VECTOR ( 'NONE', #8627, 1000.000000000000114 ) ;
#368 = ORIENTED_EDGE ( 'NONE', *, *, #2982, .T. ) ;
#369 = AXIS2_PLACEMENT_3D ( 'NONE', #12355, #9278, #12488 ) ;
#370 = VERTEX_POINT ( 'NONE', #1148 ) ;
#371 = DIRECTION ( 'NONE',  ( 0.000000000000000000, 0.000000000000000000, -1.000000000000000000 ) ) ;
#372 = ORIENTED_EDGE ( 'NONE', *, *, #5978, .T. ) ;
#373 = CARTESIAN_POINT ( 'NONE',  ( 37.09602683542106405, 121.2793079999285339, 2.999999999999998668 ) ) ;
#374 = CARTESIAN_POINT ( 'NONE',  ( 66.19999999999997442, 108.0133283987163253, 4.025000001229034119 ) ) ;
#375 = ADVANCED_FACE ( 'NONE', ( #11618, #11680 ), #2535, .T. ) ;
#376 = VERTEX_POINT ( 'NONE', #8487 ) ;
#377 = CYLINDRICAL_SURFACE ( 'NONE', #4983, 1.500000000000000222 ) ;
#378 = ORIENTED_EDGE ( 'NONE', *, *, #6492, .T. ) ;
#379 = AXIS2_PLACEMENT_3D ( 'NONE', #7414, #9573, #11532 ) ;
#380 = DIRECTION ( 'NONE',  ( -1.000000000000000000, -0.000000000000000000, -0.000000000000000000 ) ) ;
#381 = FACE_BOUND ( 'NONE', #9201, .T. ) ;
#382 = CARTESIAN_POINT ( 'NONE',  ( 60.00000000000000000, -6.000000000000000000, 15.00000000000000000 ) ) ;
#383 =( NAMED_UNIT ( * ) SI_UNIT ( $, .STERADIAN. ) SOLID_ANGLE_UNIT ( ) );
#384 = AXIS2_PLACEMENT_3D ( 'NONE', #10742, #1980, #7866 ) ;
#385 = ORIENTED_EDGE ( 'NONE', *, *, #5821, .T. ) ;
#386 = DIRECTION ( 'NONE',  ( -0.000000000000000000, 1.000000000000000000, -0.000000000000000000 ) ) ;
#387 = ORIENTED_EDGE ( 'NONE', *, *, #9281, .T. ) ;
#388 = EDGE_CURVE ( 'NONE', #12930, #2334, #4689, .T. ) ;
#389 = PLANE ( 'NONE',  #10643 ) ;
#390 = EDGE_CURVE ( 'NONE', #3842, #10632, #6639, .T. ) ;
#391 = CARTESIAN_POINT ( 'NONE',  ( 50.72178482187501203, 62.76906990284730625, 4.109375000614517326 ) ) ;
#392 = ORIENTED_EDGE ( 'NONE', *, *, #8088, .T. ) ;
#393 = CIRCLE ( 'NONE', #7723, 4.000000000000003553 ) ;
#394 = CARTESIAN_POINT ( 'NONE',  ( 33.50000000000000711, 67.79999999999999716, 8.000000000000000000 ) ) ;
#395 = CARTESIAN_POINT ( 'NONE',  ( 3.591865698314129496, 91.49237114305354623, 2.999999999999999556 ) ) ;
#396 = CARTESIAN_POINT ( 'NONE',  ( 19.27821517812503060, 62.76906990284727783, 3.134375000614517237 ) ) ;
#397 = CARTESIAN_POINT ( 'NONE',  ( 0.000000000000000000, 0.000000000000000000, -0.8000000000000000444 ) ) ;
#398 = LINE ( 'NONE', #10557, #7920 ) ;
#399 = CARTESIAN_POINT ( 'NONE',  ( 38.40477530926830951, 84.46307801270444315, -1.000000000000000000 ) ) ;
#400 = AXIS2_PLACEMENT_3D ( 'NONE', #292, #2539, #8422 ) ;
#401 = CARTESIAN_POINT ( 'NONE',  ( 48.49999999999995737, 94.00000000000000000, -8.000000000000000000 ) ) ;
#402 = CARTESIAN_POINT ( 'NONE',  ( 1.750000000000000000, 0.000000000000000000, 0.000000000000000000 ) ) ;
#403 = CARTESIAN_POINT ( 'NONE',  ( 35.00000000000000000, 90.00000000000000000, 4.800000000000000711 ) ) ;
#404 = DIRECTION ( 'NONE',  ( 0.000000000000000000, 0.000000000000000000, -1.000000000000000000 ) ) ;
#405 = CARTESIAN_POINT ( 'NONE',  ( 37.99038105676688559, 21.93375672974103452, 1.000000000000000000 ) ) ;
#406 = LINE ( 'NONE', #4420, #3286 ) ;
#407 = ADVANCED_FACE ( 'NONE', ( #2595 ), #7436, .F. ) ;
#408 = VERTEX_POINT ( 'NONE', #12543 ) ;
#409 = CARTESIAN_POINT ( 'NONE',  ( 25.00000000000000000, 90.00000000000000000, -10.00000000000000000 ) ) ;
#410 = AXIS2_PLACEMENT_3D ( 'NONE', #10816, #609, #2848 ) ;
#411 = DIRECTION ( 'NONE',  ( -0.000000000000000000, 1.000000000000000000, -0.000000000000000000 ) ) ;
#412 = ORIENTED_EDGE ( 'NONE', *, *, #1216, .T. ) ;
#413 =( LENGTH_UNIT ( ) NAMED_UNIT ( * ) SI_UNIT ( .MILLI., .METRE. ) );
#414 = DIRECTION ( 'NONE',  ( 0.000000000000000000, 0.000000000000000000, -1.000000000000000000 ) ) ;
#415 = CARTESIAN_POINT ( 'NONE',  ( 50.60000000000001563, 62.98000740192552627, 4.362500001229034474 ) ) ;
#416 = CARTESIAN_POINT ( 'NONE',  ( 35.00000000000000000, 90.00000000000000000, 4.000000000000000000 ) ) ;
#417 = CIRCLE ( 'NONE', #3994, 3.499999999999996003 ) ;
#418 = ORIENTED_EDGE ( 'NONE', *, *, #1473, .F. ) ;
#419 = EDGE_CURVE ( 'NONE', #6987, #1436, #9061, .T. ) ;
#420 = FACE_OUTER_BOUND ( 'NONE', #4531, .T. ) ;
#421 = CARTESIAN_POINT ( 'NONE',  ( 0.000000000000000000, 0.5773502691896263972, -1.000000000000000000 ) ) ;
#422 = EDGE_CURVE ( 'NONE', #998, #10285, #11419, .T. ) ;
#423 = EDGE_LOOP ( 'NONE', ( #4044, #8845, #2488, #12293, #6036, #11034 ) ) ;
#424 = SHAPE_REPRESENTATION_RELATIONSHIP ( 'NONE' , 'NONE' ,  #9523, #10270 ) ;
#425 = CARTESIAN_POINT ( 'NONE',  ( -18.00412335955691745, 88.33754051161746190, 1.000000000000003109 ) ) ;
#426 = EDGE_CURVE ( 'NONE', #11653, #6806, #2729, .T. ) ;
#427 = VERTEX_POINT ( 'NONE', #1412 ) ;
#428 = CARTESIAN_POINT ( 'NONE',  ( 66.44356964374999563, 90.00000000000000000, 3.228125000614517237 ) ) ;
#429 = EDGE_LOOP ( 'NONE', ( #3770, #8264, #6534, #4530, #5902, #2222, #1505, #1439 ) ) ;
#430 = DIRECTION ( 'NONE',  ( -5.624500927088228034E-17, 1.370729058197317775E-18, 1.000000000000000000 ) ) ;
#431 = AXIS2_PLACEMENT_3D ( 'NONE', #2573, #8714, #3560 ) ;
#432 = DIRECTION ( 'NONE',  ( 0.000000000000000000, 0.000000000000000000, 1.000000000000000000 ) ) ;
#433 = ORIENTED_EDGE ( 'NONE', *, *, #4981, .F. ) ;
#434 = ORIENTED_EDGE ( 'NONE', *, *, #4950, .T. ) ;
#435 = CARTESIAN_POINT ( 'NONE',  ( 40.00000000000000000, 0.000000000000000000, 10.00000000000000000 ) ) ;
#436 = ORIENTED_EDGE ( 'NONE', *, *, #12848, .T. ) ;
#437 = CARTESIAN_POINT ( 'NONE',  ( 60.02959220194507139, 108.7322598613235414, 2.999999999999999556 ) ) ;
#438 = CONTEXT_DEPENDENT_SHAPE_REPRESENTATION ( #4763, #825 ) ;
#439 = CARTESIAN_POINT ( 'NONE',  ( 3.800000000000015365, 108.0133283987163111, 3.725000001229034297 ) ) ;
#440 = EDGE_CURVE ( 'NONE', #7916, #8087, #6573, .T. ) ;
#441 = EDGE_LOOP ( 'NONE', ( #236, #7328, #3929 ) ) ;
#442 = CIRCLE ( 'NONE', #5674, 30.00000000000000000 ) ;
#443 = VERTEX_POINT ( 'NONE', #483 ) ;
#444 = CARTESIAN_POINT ( 'NONE',  ( 35.00000000000000000, 90.00000000000000000, 4.000000000000000000 ) ) ;
#445 = ORIENTED_EDGE ( 'NONE', *, *, #1486, .T. ) ;
#446 = CARTESIAN_POINT ( 'NONE',  ( 0.000000000000000000, 2.000000000000000000, 0.000000000000000000 ) ) ;
#447 = DIRECTION ( 'NONE',  ( 0.000000000000000000, 0.000000000000000000, -1.000000000000000000 ) ) ;
#448 = VECTOR ( 'NONE', #5301, 1000.000000000000000 ) ;
#449 = ORIENTED_EDGE ( 'NONE', *, *, #16, .T. ) ;
#450 = PLANE ( 'NONE',  #6571 ) ;
#451 = VERTEX_POINT ( 'NONE', #10505 ) ;
#452 = DIRECTION ( 'NONE',  ( -0.000000000000000000, -1.000000000000000000, -0.000000000000000000 ) ) ;
#453 = EDGE_CURVE ( 'NONE', #9165, #12799, #1651, .T. ) ;
#454 = VERTEX_POINT ( 'NONE', #7693 ) ;
#455 = CARTESIAN_POINT ( 'NONE',  ( 64.54728994471078352, 100.7543353520590870, 2.858851390178780871 ) ) ;
#456 = ORIENTED_EDGE ( 'NONE', *, *, #7665, .T. ) ;
#457 = AXIS2_PLACEMENT_3D ( 'NONE', #11629, #9541, #8624 ) ;
#458 = DIRECTION ( 'NONE',  ( 0.000000000000000000, -0.000000000000000000, 1.000000000000000000 ) ) ;
#459 = DIRECTION ( 'NONE',  ( 0.000000000000000000, 0.000000000000000000, -1.000000000000000000 ) ) ;
#460 = CARTESIAN_POINT ( 'NONE',  ( 66.44356964375000985, 71.84604660189820891, 4.146875000614517859 ) ) ;
#461 = CARTESIAN_POINT ( 'NONE',  ( 40.00000000000000000, 0.000000000000000000, -10.00000000000000000 ) ) ;
#462 = EDGE_CURVE ( 'NONE', #12941, #5885, #2810, .T. ) ;
#463 = DIRECTION ( 'NONE',  ( -0.000000000000000000, -0.000000000000000000, 1.000000000000000000 ) ) ;
#464 = EDGE_CURVE ( 'NONE', #9403, #7005, #12208, .T. ) ;
#465 = DIRECTION ( 'NONE',  ( 0.000000000000000000, 0.000000000000000000, -1.000000000000000000 ) ) ;
#466 =( GEOMETRIC_REPRESENTATION_CONTEXT ( 3 ) GLOBAL_UNCERTAINTY_ASSIGNED_CONTEXT ( ( #584 ) ) GLOBAL_UNIT_ASSIGNED_CONTEXT ( ( #1408, #547, #9650 ) ) REPRESENTATION_CONTEXT ( 'NONE', 'WORKASPACE' ) );
#467 = FACE_OUTER_BOUND ( 'NONE', #11124, .T. ) ;
#468 = DIRECTION ( 'NONE',  ( 1.000000000000000000, 0.000000000000000000, 0.000000000000000000 ) ) ;
#469 = DIRECTION ( 'NONE',  ( -0.000000000000000000, 1.000000000000000000, -0.000000000000000000 ) ) ;
#470 = VECTOR ( 'NONE', #11203, 1000.000000000000000 ) ;
#471 = ADVANCED_FACE ( 'NONE', ( #3454, #10443, #9457 ), #4494, .T. ) ;
#472 = CARTESIAN_POINT ( 'NONE',  ( 35.00000000000000000, 90.00000000000000000, -8.000000000000000000 ) ) ;
#473 = CARTESIAN_POINT ( 'NONE',  ( 35.00000000000000000, 126.0266567974326222, 4.887499999999999289 ) ) ;
#474 = DIRECTION ( 'NONE',  ( -0.8660254037844360431, -0.5000000000000047740, -0.000000000000000000 ) ) ;
#475 = ORIENTED_EDGE ( 'NONE', *, *, #517, .T. ) ;
#476 = PLANE ( 'NONE',  #4013 ) ;
#477 = CARTESIAN_POINT ( 'NONE',  ( -28.99038105676692112, 50.21281292110204930, -1.000000000000000000 ) ) ;
#478 = ORIENTED_EDGE ( 'NONE', *, *, #11274, .T. ) ;
#479 = CIRCLE ( 'NONE', #1327, 28.99999999999999289 ) ;
#480 = CARTESIAN_POINT ( 'NONE',  ( 3.800000000000004707, 90.00000000000000000, 6.000000000000000000 ) ) ;
#481 = CARTESIAN_POINT ( 'NONE',  ( 8.999999999999989342, 72.14656965084313356, -1.000000000000000000 ) ) ;
#482 = ADVANCED_FACE ( 'NONE', ( #1540, #5532 ), #12604, .F. ) ;
#483 = CARTESIAN_POINT ( 'NONE',  ( 4.999999999999962697, 79.07477288111861924, 3.000000000000000000 ) ) ;
#484 = ORIENTED_EDGE ( 'NONE', *, *, #7097, .F. ) ;
#485 = VERTEX_POINT ( 'NONE', #3968 ) ;
#486 = DIRECTION ( 'NONE',  ( 4.336808689942017243E-16, 2.503857664561960972E-16, -1.000000000000000000 ) ) ;
#487 = DIRECTION ( 'NONE',  ( -0.000000000000000000, 1.000000000000000000, -0.000000000000000000 ) ) ;
#488 = VERTEX_POINT ( 'NONE', #6898 ) ;
#489 = DIRECTION ( 'NONE',  ( 0.000000000000000000, 0.000000000000000000, 1.000000000000000000 ) ) ;
#490 = AXIS2_PLACEMENT_3D ( 'NONE', #552, #3647, #7627 ) ;
#491 = CARTESIAN_POINT ( 'NONE',  ( 35.00000000000000000, 90.00000000000000000, -0.9999999999999970024 ) ) ;
#492 = ORIENTED_EDGE ( 'NONE', *, *, #5266, .F. ) ;
#493 =( GEOMETRIC_REPRESENTATION_CONTEXT ( 3 ) GLOBAL_UNCERTAINTY_ASSIGNED_CONTEXT ( ( #8293 ) ) GLOBAL_UNIT_ASSIGNED_CONTEXT ( ( #12067, #10294, #5125 ) ) REPRESENTATION_CONTEXT ( 'NONE', 'WORKASPACE' ) );
#494 = DIRECTION ( 'NONE',  ( 1.000000000000000000, 0.000000000000000000, 0.000000000000000000 ) ) ;
#495 = ORIENTED_EDGE ( 'NONE', *, *, #4508, .T. ) ;
#496 = LINE ( 'NONE', #7448, #8208 ) ;
#497 = LINE ( 'NONE', #6524, #12081 ) ;
#498 = ORIENTED_EDGE ( 'NONE', *, *, #4803, .F. ) ;
#499 = AXIS2_PLACEMENT_3D ( 'NONE', #6594, #5619, #11504 ) ;
#500 = EDGE_CURVE ( 'NONE', #6408, #3143, #4030, .T. ) ;
#501 = ORIENTED_EDGE ( 'NONE', *, *, #9357, .T. ) ;
#502 = AXIS2_PLACEMENT_3D ( 'NONE', #7934, #12717, #11921 ) ;
#503 = DIRECTION ( 'NONE',  ( -0.000000000000000000, -0.000000000000000000, -1.000000000000000000 ) ) ;
#504 = ORIENTED_EDGE ( 'NONE', *, *, #2993, .F. ) ;
#505 = CARTESIAN_POINT ( 'NONE',  ( 9.369499999999998607, 0.000000000000000000, 0.000000000000000000 ) ) ;
#506 = CONTEXT_DEPENDENT_SHAPE_REPRESENTATION ( #6758, #8984 ) ;
#507 = LINE ( 'NONE', #4515, #8154 ) ;
#508 = ORIENTED_EDGE ( 'NONE', *, *, #9196, .T. ) ;
#509 = CARTESIAN_POINT ( 'NONE',  ( -2.387319993259524598, -4.036502139894371233, 0.000000000000000000 ) ) ;
#510 = ORIENTED_EDGE ( 'NONE', *, *, #7411, .F. ) ;
#511 = CARTESIAN_POINT ( 'NONE',  ( -6.666666666666660745, 0.000000000000000000, 0.000000000000000000 ) ) ;
#513 = ORIENTED_EDGE ( 'NONE', *, *, #12102, .F. ) ;
#512 = VECTOR ( 'NONE', #6257, 1000.000000000000000 ) ;
#514 = CARTESIAN_POINT ( 'NONE',  ( 66.19999999999988916, 71.98667160128361786, 4.287500000000000533 ) ) ;
#515 = CARTESIAN_POINT ( 'NONE',  ( -3.068288344391240763, -2.655262421758692426, -0.8000000000000000444 ) ) ;
#516 = EDGE_CURVE ( 'NONE', #767, #10706, #9716, .T. ) ;
#517 = EDGE_CURVE ( 'NONE', #7067, #10542, #2603, .T. ) ;
#518 = EDGE_LOOP ( 'NONE', ( #12338, #1240, #6550, #7565 ) ) ;
#519 = CARTESIAN_POINT ( 'NONE',  ( 60.63303221600038739, 111.5086687461494392, 2.885734441893565538 ) ) ;
#520 = ORIENTED_EDGE ( 'NONE', *, *, #6993, .F. ) ;
#521 = VECTOR ( 'NONE', #8150, 1000.000000000000000 ) ;
#522 = DIRECTION ( 'NONE',  ( -0.000000000000000000, -1.000000000000000000, -0.000000000000000000 ) ) ;
#523 = VECTOR ( 'NONE', #11793, 1000.000000000000000 ) ;
#524 = ORIENTED_EDGE ( 'NONE', *, *, #12861, .T. ) ;
#525 = CARTESIAN_POINT ( 'NONE',  ( 3.556430356250015024, 90.00000000000000000, 3.959375000614517415 ) ) ;
#526 = ORIENTED_EDGE ( 'NONE', *, *, #10407, .T. ) ;
#527 = CARTESIAN_POINT ( 'NONE',  ( 3.800000000000015365, 90.00000000000000000, 4.100000000000000533 ) ) ;
#528 = CARTESIAN_POINT ( 'NONE',  ( 3.737990899702874348, 93.52352325000568101, 3.000000000000000000 ) ) ;
#529 = CARTESIAN_POINT ( 'NONE',  ( 1.040000000000000036, 0.000000000000000000, 0.000000000000000000 ) ) ;
#530 = AXIS2_PLACEMENT_3D ( 'NONE', #7357, #8344, #1205 ) ;
#531 = EDGE_CURVE ( 'NONE', #3957, #12821, #1005, .T. ) ;
#532 = CARTESIAN_POINT ( 'NONE',  ( 64.85903780527353035, 87.09520029206045422, -3.000000000000000000 ) ) ;
#533 = VECTOR ( 'NONE', #6646, 1000.000000000000000 ) ;
#534 = DIRECTION ( 'NONE',  ( 0.4999999999999987232, -0.8660254037844393737, 0.000000000000000000 ) ) ;
#535 = DIRECTION ( 'NONE',  ( -5.624500927088228034E-17, 1.370729058197317968E-18, 1.000000000000000000 ) ) ;
#536 = LINE ( 'NONE', #736, #3548 ) ;
#537 = LINE ( 'NONE', #1464, #10952 ) ;
#538 = CARTESIAN_POINT ( 'NONE',  ( 3.033375984251970081, -8.673617379884035472E-16, 0.000000000000000000 ) ) ;
#539 = EDGE_CURVE ( 'NONE', #7517, #3017, #9903, .T. ) ;
#540 = AXIS2_PLACEMENT_3D ( 'NONE', #1275, #10104, #5264 ) ;
#541 = DIRECTION ( 'NONE',  ( 0.000000000000000000, 0.000000000000000000, 1.000000000000000000 ) ) ;
#542 = CARTESIAN_POINT ( 'NONE',  ( 19.40000000000000924, 117.0199925980744666, 3.687500001229034208 ) ) ;
#543 = ORIENTED_EDGE ( 'NONE', *, *, #11638, .F. ) ;
#544 = LINE ( 'NONE', #8546, #10 ) ;
#545 = CARTESIAN_POINT ( 'NONE',  ( 1.617350269189632428, 0.000000000000000000, 0.000000000000000000 ) ) ;
#546 = ORIENTED_EDGE ( 'NONE', *, *, #10576, .T. ) ;
#547 =( NAMED_UNIT ( * ) PLANE_ANGLE_UNIT ( ) SI_UNIT ( $, .RADIAN. ) );
#548 = ADVANCED_FACE ( 'NONE', ( #11812, #12733 ), #8016, .F. ) ;
#549 = VECTOR ( 'NONE', #1621, 1000.000000000000000 ) ;
#550 = DIRECTION ( 'NONE',  ( 0.000000000000000000, -1.000000000000000000, 0.000000000000000000 ) ) ;
#551 = DIRECTION ( 'NONE',  ( -0.000000000000000000, -1.000000000000000000, -0.000000000000000000 ) ) ;
#552 = CARTESIAN_POINT ( 'NONE',  ( 35.00000000000000000, 90.00000000000000000, 6.000000000000000000 ) ) ;
#553 = ORIENTED_EDGE ( 'NONE', *, *, #4093, .T. ) ;
#554 = DIRECTION ( 'NONE',  ( 0.000000000000000000, 0.000000000000000000, 1.000000000000000000 ) ) ;
#555 = CARTESIAN_POINT ( 'NONE',  ( 0.1038759689922479496, -3.348389132562988646, -0.8000000000000000444 ) ) ;
#556 = ADVANCED_FACE ( 'NONE', ( #3049, #10826 ), #5003, .F. ) ;
#557 = ORIENTED_EDGE ( 'NONE', *, *, #7447, .F. ) ;
#558 = CARTESIAN_POINT ( 'NONE',  ( 35.00000000000000000, 90.00000000000000000, 4.000000000000000000 ) ) ;
#559 = DIRECTION ( 'NONE',  ( 1.000000000000000000, -0.000000000000000000, 0.000000000000000000 ) ) ;
#560 = ORIENTED_EDGE ( 'NONE', *, *, #12372, .T. ) ;
#561 = VECTOR ( 'NONE', #4344, 999.9999999999998863 ) ;
#562 = FACE_OUTER_BOUND ( 'NONE', #1188, .T. ) ;
#563 = ORIENTED_EDGE ( 'NONE', *, *, #5905, .F. ) ;
#564 = CARTESIAN_POINT ( 'NONE',  ( 45.39999948872177526, 60.58435772187547030, 3.000000000000000000 ) ) ;
#565 = FACE_OUTER_BOUND ( 'NONE', #1775, .T. ) ;
#566 = ORIENTED_EDGE ( 'NONE', *, *, #10069, .F. ) ;
#567 = FACE_OUTER_BOUND ( 'NONE', #6153, .T. ) ;
#568 = ORIENTED_EDGE ( 'NONE', *, *, #10862, .T. ) ;
#569 = AXIS2_PLACEMENT_3D ( 'NONE', #2591, #4682, #2724 ) ;
#570 = CARTESIAN_POINT ( 'NONE',  ( 8.499999999999998224, 79.07477288111861924, 1.000000000000000000 ) ) ;
#571 = VERTEX_POINT ( 'NONE', #2859 ) ;
#572 = DIRECTION ( 'NONE',  ( -1.000000000000000000, 0.000000000000000000, 0.000000000000000000 ) ) ;
#573 = SHAPE_DEFINITION_REPRESENTATION ( #2509, #985 ) ;
#574 = CARTESIAN_POINT ( 'NONE',  ( 3.800000000000015365, 90.00000000000000000, 3.200000000000000178 ) ) ;
#575 = ORIENTED_EDGE ( 'NONE', *, *, #4120, .F. ) ;
#576 = ORIENTED_EDGE ( 'NONE', *, *, #12211, .T. ) ;
#577 = SURFACE_STYLE_FILL_AREA ( #1504 ) ;
#578 = ORIENTED_EDGE ( 'NONE', *, *, #7988, .T. ) ;
#579 = ADVANCED_FACE ( 'NONE', ( #1999 ), #8988, .F. ) ;
#580 = VECTOR ( 'NONE', #12744, 1000.000000000000000 ) ;
#581 = AXIS2_PLACEMENT_3D ( 'NONE', #6283, #2043, #10989 ) ;
#582 = CARTESIAN_POINT ( 'NONE',  ( 35.39078165856646763, 58.73470357045291479, 3.000000000000001332 ) ) ;
#583 = DIRECTION ( 'NONE',  ( -1.000000000000000000, 0.000000000000000000, 0.000000000000000000 ) ) ;
#584 = UNCERTAINTY_MEASURE_WITH_UNIT (LENGTH_MEASURE( 1.000000000000000082E-05 ), #1408, 'distance_accuracy_value', 'NONE');
#585 = VERTEX_POINT ( 'NONE', #1932 ) ;
#586 = CARTESIAN_POINT ( 'NONE',  ( 35.00000000000000711, 53.69209320379640360, 3.621875000614517059 ) ) ;
#587 = VERTEX_POINT ( 'NONE', #749 ) ;
#588 = PLANE ( 'NONE',  #11054 ) ;
#589 = VECTOR ( 'NONE', #11996, 1000.000000000000000 ) ;
#590 = ORIENTED_EDGE ( 'NONE', *, *, #5677, .T. ) ;
#591 = CARTESIAN_POINT ( 'NONE',  ( 3.556430356250015024, 90.00000000000000000, 3.509375000614517681 ) ) ;
#592 = ORIENTED_EDGE ( 'NONE', *, *, #5905, .T. ) ;
#593 = ADVANCED_FACE ( 'NONE', ( #5912, #5791 ), #3774, .T. ) ;
#594 = CARTESIAN_POINT ( 'NONE',  ( 66.20000000000004547, 108.0133283987162969, 3.912500000000000977 ) ) ;
#595 = DIRECTION ( 'NONE',  ( -0.000000000000000000, -1.000000000000000000, -0.000000000000000000 ) ) ;
#596 = EDGE_CURVE ( 'NONE', #330, #4076, #4069, .T. ) ;
#597 = DIRECTION ( 'NONE',  ( -0.000000000000000000, -1.000000000000000000, -0.000000000000000000 ) ) ;
#598 = CARTESIAN_POINT ( 'NONE',  ( 0.000000000000000000, -0.5773502691896256200, -1.000000000000000000 ) ) ;
#600 = AXIS2_PLACEMENT_3D ( 'NONE', #4155, #337, #1325 ) ;
#599 = DIRECTION ( 'NONE',  ( 1.000000000000000000, 0.000000000000000000, 0.000000000000000000 ) ) ;
#601 = DIRECTION ( 'NONE',  ( -0.000000000000000000, 1.000000000000000000, -0.000000000000000000 ) ) ;
#602 = CARTESIAN_POINT ( 'NONE',  ( 35.00000000000000000, 90.00000000000000000, -0.9999999999999970024 ) ) ;
#603 = DIRECTION ( 'NONE',  ( 0.000000000000000000, 0.5150380737757253025, 0.8571673013836857979 ) ) ;
#604 = CARTESIAN_POINT ( 'NONE',  ( -6.666666666666660745, 2.000000000000001332, -1.599999999999986766 ) ) ;
#605 = VECTOR ( 'NONE', #12118, 1000.000000000000000 ) ;
#606 = FACE_OUTER_BOUND ( 'NONE', #6514, .T. ) ;
#607 = ADVANCED_FACE ( 'NONE', ( #809 ), #12923, .T. ) ;
#608 = VECTOR ( 'NONE', #6526, 1000.000000000000000 ) ;
#609 = DIRECTION ( 'NONE',  ( -1.000000000000000000, -0.000000000000000000, -0.000000000000000000 ) ) ;
#610 = CARTESIAN_POINT ( 'NONE',  ( 35.00000000000000000, 90.00000000000000000, -1.000000000000000000 ) ) ;
#611 = ORIENTED_EDGE ( 'NONE', *, *, #2370, .T. ) ;
#612 = CARTESIAN_POINT ( 'NONE',  ( 50.59999999999999432, 117.0199925980744666, 4.400000000000000355 ) ) ;
#613 = LINE ( 'NONE', #545, #2256 ) ;
#614 = ORIENTED_EDGE ( 'NONE', *, *, #6666, .F. ) ;
#615 =( NAMED_UNIT ( * ) SI_UNIT ( $, .STERADIAN. ) SOLID_ANGLE_UNIT ( ) );
#616 = VECTOR ( 'NONE', #1823, 1000.000000000000000 ) ;
#617 = DIRECTION ( 'NONE',  ( 1.000000000000000000, 0.000000000000000000, 0.000000000000000000 ) ) ;
#618 = CARTESIAN_POINT ( 'NONE',  ( 48.11036777325283964, 61.54261756562988239, 3.006515308376277229 ) ) ;
#619 = VERTEX_POINT ( 'NONE', #8800 ) ;
#620 = PLANE ( 'NONE',  #2626 ) ;
#621 = CARTESIAN_POINT ( 'NONE',  ( 19.27821517812503060, 62.76906990284727783, 4.428125000614516971 ) ) ;
#622 = EDGE_CURVE ( 'NONE', #3150, #9073, #1826, .T. ) ;
#623 = ORIENTED_EDGE ( 'NONE', *, *, #10337, .T. ) ;
#624 = AXIS2_PLACEMENT_3D ( 'NONE', #12004, #1206, #5133 ) ;
#625 = DIRECTION ( 'NONE',  ( -0.8746197064978278313, 0.4848096214037562746, 1.049727191973305270E-16 ) ) ;
#626 =( NAMED_UNIT ( * ) SI_UNIT ( $, .STERADIAN. ) SOLID_ANGLE_UNIT ( ) );
#627 = ORIENTED_EDGE ( 'NONE', *, *, #322, .T. ) ;
#628 = LINE ( 'NONE', #4760, #11001 ) ;
#629 = ORIENTED_EDGE ( 'NONE', *, *, #7794, .T. ) ;
#630 = CARTESIAN_POINT ( 'NONE',  ( 18.35873618070580093, 66.24461453698026503, 4.000000000000000000 ) ) ;
#631 = CYLINDRICAL_SURFACE ( 'NONE', #12303, 0.9999999999999991118 ) ;
#632 = EDGE_CURVE ( 'NONE', #11636, #4911, #11998, .T. ) ;
#633 = ADVANCED_FACE ( 'NONE', ( #3905 ), #2920, .F. ) ;
#634 = CIRCLE ( 'NONE', #12768, 3.350000000000000089 ) ;
#635 = DIRECTION ( 'NONE',  ( -1.000000000000000000, 0.000000000000000000, 0.000000000000000000 ) ) ;
#636 = CARTESIAN_POINT ( 'NONE',  ( 35.75000000000000711, 92.49999999999998579, -3.000000000000000000 ) ) ;
#637 = DIRECTION ( 'NONE',  ( 0.000000000000000000, 0.000000000000000000, -1.000000000000000000 ) ) ;
#638 = ORIENTED_EDGE ( 'NONE', *, *, #97, .F. ) ;
#639 = DIRECTION ( 'NONE',  ( -1.000000000000000000, -0.000000000000000000, -0.000000000000000000 ) ) ;
#640 = CONTEXT_DEPENDENT_SHAPE_REPRESENTATION ( #11014, #5527 ) ;
#641 = CARTESIAN_POINT ( 'NONE',  ( 19.40000000000002700, 62.98000740192551206, 3.837500001229034563 ) ) ;
#642 = ORIENTED_EDGE ( 'NONE', *, *, #5141, .F. ) ;
#643 = SURFACE_STYLE_USAGE ( .BOTH. , #9675 ) ;
#644 = ORIENTED_EDGE ( 'NONE', *, *, #5801, .F. ) ;
#645 = VECTOR ( 'NONE', #10208, 1000.000000000000227 ) ;
#646 = DIRECTION ( 'NONE',  ( 0.000000000000000000, 0.000000000000000000, 1.000000000000000000 ) ) ;
#647 = EDGE_LOOP ( 'NONE', ( #10608, #8614 ) ) ;
#648 = CARTESIAN_POINT ( 'NONE',  ( 15.29066239423023887, 65.64213830996915533, 3.000000000000000444 ) ) ;
#649 = LINE ( 'NONE', #2821, #9778 ) ;
#650 = ORIENTED_EDGE ( 'NONE', *, *, #2075, .F. ) ;
#651 = CARTESIAN_POINT ( 'NONE',  ( 64.54728993811707483, 100.7543353701752125, 2.858851390224067313 ) ) ;
#652 = EDGE_LOOP ( 'NONE', ( #3973, #10053 ) ) ;
#653 = EDGE_CURVE ( 'NONE', #6728, #2032, #6175, .T. ) ;
#654 = CARTESIAN_POINT ( 'NONE',  ( -60.00000000000000000, 30.00000000000000000, 2.500000000000000000 ) ) ;
#655 = VERTEX_POINT ( 'NONE', #9185 ) ;
#656 = CARTESIAN_POINT ( 'NONE',  ( 50.72178482187501203, 62.76906990284730625, 3.209375000614517415 ) ) ;
#657 = ORIENTED_EDGE ( 'NONE', *, *, #9994, .T. ) ;
#658 = DIRECTION ( 'NONE',  ( 0.000000000000000000, -1.000000000000000000, 0.000000000000000000 ) ) ;
#659 = CARTESIAN_POINT ( 'NONE',  ( 6.499999999999999112, 68.39379290111055809, 2.999999999999960032 ) ) ;
#660 = FACE_OUTER_BOUND ( 'NONE', #1254, .T. ) ;
#661 = AXIS2_PLACEMENT_3D ( 'NONE', #10121, #1470, #8480 ) ;
#662 = CARTESIAN_POINT ( 'NONE',  ( 19.27821517812500574, 117.2309300971526937, 4.728125000614516793 ) ) ;
#663 = EDGE_CURVE ( 'NONE', #698, #11775, #6107, .T. ) ;
#664 = DIRECTION ( 'NONE',  ( -0.000000000000000000, -0.000000000000000000, -1.000000000000000000 ) ) ;
#665 = CARTESIAN_POINT ( 'NONE',  ( 35.00000000000000000, 90.00000000000000000, 4.000000000000000000 ) ) ;
#666 = EDGE_CURVE ( 'NONE', #8482, #12120, #12330, .T. ) ;
#667 = CARTESIAN_POINT ( 'NONE',  ( -54.07179676972453564, 35.73205080756890339, -1.000000000000000000 ) ) ;
#668 = DIRECTION ( 'NONE',  ( 0.000000000000000000, 1.000000000000000000, -1.370729058197317775E-18 ) ) ;
#669 = VECTOR ( 'NONE', #1046, 1000.000000000000000 ) ;
#670 = PLANE ( 'NONE',  #6171 ) ;
#671 = DIRECTION ( 'NONE',  ( 0.8660254037844361541, 0.5000000000000042188, 0.000000000000000000 ) ) ;
#672 = CARTESIAN_POINT ( 'NONE',  ( 66.44356964374998142, 108.1539533981018053, 3.771875000614516971 ) ) ;
#673 = ORIENTED_EDGE ( 'NONE', *, *, #3401, .T. ) ;
#674 = DIRECTION ( 'NONE',  ( -0.000000000000000000, 1.000000000000000000, -0.000000000000000000 ) ) ;
#675 = DIRECTION ( 'NONE',  ( 5.624500927088228034E-17, -1.370729058197317775E-18, -1.000000000000000000 ) ) ;
#676 = ORIENTED_EDGE ( 'NONE', *, *, #11289, .T. ) ;
#677 = VECTOR ( 'NONE', #9665, 1000.000000000000000 ) ;
#678 = EDGE_CURVE ( 'NONE', #12162, #3526, #8342, .T. ) ;
#679 = DIRECTION ( 'NONE',  ( 0.9510565162951554186, -0.3090169943749414005, 0.000000000000000000 ) ) ;
#680 = DIRECTION ( 'NONE',  ( 1.000000000000000000, 0.000000000000000000, -0.000000000000000000 ) ) ;
#681 = VERTEX_POINT ( 'NONE', #7030 ) ;
#682 = CARTESIAN_POINT ( 'NONE',  ( 7.500000000000000000, 30.00000000000000000, 0.000000000000000000 ) ) ;
#683 = CARTESIAN_POINT ( 'NONE',  ( 66.44356964374998142, 108.1539533981018053, 3.715625000614517948 ) ) ;
#684 = COLOUR_RGB ( '',0.8941176470588234615, 0.8941176470588234615, 0.8941176470588234615 ) ;
#685 = DIRECTION ( 'NONE',  ( -0.8660254037844361541, -0.5000000000000042188, 9.389466242107218061E-17 ) ) ;
#686 = DIRECTION ( 'NONE',  ( 0.000000000000000000, 0.000000000000000000, 1.000000000000000000 ) ) ;
#687 = ORIENTED_EDGE ( 'NONE', *, *, #453, .F. ) ;
#688 = CARTESIAN_POINT ( 'NONE',  ( 7.500000000000000000, 27.00000000000000000, 0.000000000000000000 ) ) ;
#689 = ORIENTED_EDGE ( 'NONE', *, *, #1063, .F. ) ;
#690 = VECTOR ( 'NONE', #8750, 1000.000000000000114 ) ;
#691 = CARTESIAN_POINT ( 'NONE',  ( 25.00000000000000355, 0.000000000000000000, 4.249999999999998224 ) ) ;
#692 = LINE ( 'NONE', #4702, #11877 ) ;
#693 = EDGE_CURVE ( 'NONE', #12083, #4963, #12636, .T. ) ;
#694 = PRESENTATION_LAYER_ASSIGNMENT (  '', '', ( #11566 ) ) ;
#695 = LINE ( 'NONE', #11320, #4590 ) ;
#696 = ORIENTED_EDGE ( 'NONE', *, *, #6826, .F. ) ;
#697 = CARTESIAN_POINT ( 'NONE',  ( 0.000000000000000000, 2.000000000000000000, 0.000000000000000000 ) ) ;
#698 = VERTEX_POINT ( 'NONE', #11012 ) ;
#699 = CLOSED_SHELL ( 'NONE', ( #4681, #2294, #5712, #12137, #6395, #6284, #10454, #6271, #7033, #8769, #9664, #6996, #3078, #6506, #5758, #9872, #10478, #5588, #2469, #1397, #4829, #5175, #6473, #11028, #2843, #8926, #11939, #3918, #407, #9755, #9220, #11801, #9117, #7996, #2544, #5940, #1715, #12395, #866, #5366, #1669, #7054, #12542, #2318, #6182, #10197, #10507 ) ) ;
#700 = DIRECTION ( 'NONE',  ( 0.000000000000000000, 1.000000000000000000, 0.000000000000000000 ) ) ;
#701 = CONTEXT_DEPENDENT_SHAPE_REPRESENTATION ( #4097, #203 ) ;
#702 = CARTESIAN_POINT ( 'NONE',  ( 0.000000000000000000, 0.000000000000000000, 1.499999999999999556 ) ) ;
#703 = VERTEX_POINT ( 'NONE', #4159 ) ;
#704 = CARTESIAN_POINT ( 'NONE',  ( 35.00000000000000000, 90.00000000000000000, -10.00000000000000000 ) ) ;
#705 = EDGE_CURVE ( 'NONE', #12083, #370, #10296, .T. ) ;
#706 = ORIENTED_EDGE ( 'NONE', *, *, #3432, .T. ) ;
#707 = EDGE_CURVE ( 'NONE', #1672, #10599, #4291, .T. ) ;
#708 = PRODUCT_DEFINITION_FORMATION_WITH_SPECIFIED_SOURCE ( 'ANY', '', #2726, .NOT_KNOWN. ) ;
#709 = LINE ( 'NONE', #2754, #11300 ) ;
#710 = ORIENTED_EDGE ( 'NONE', *, *, #10661, .T. ) ;
#711 = DIRECTION ( 'NONE',  ( 0.000000000000000000, 0.5150380737757253025, 0.8571673013836857979 ) ) ;
#712 = LINE ( 'NONE', #12759, #4156 ) ;
#713 = AXIS2_PLACEMENT_3D ( 'NONE', #1399, #12460, #4544 ) ;
#714 = AXIS2_PLACEMENT_3D ( 'NONE', #11287, #12341, #11156 ) ;
#715 = ADVANCED_FACE ( 'NONE', ( #10234 ), #11079, .T. ) ;
#716 = VERTEX_POINT ( 'NONE', #3314 ) ;
#717 = DIRECTION ( 'NONE',  ( 0.000000000000000000, 0.000000000000000000, 1.000000000000000000 ) ) ;
#718 = VERTEX_POINT ( 'NONE', #4225 ) ;
#719 = FACE_OUTER_BOUND ( 'NONE', #6790, .T. ) ;
#720 = EDGE_LOOP ( 'NONE', ( #4308, #11552, #5164, #9758 ) ) ;
#721 = CIRCLE ( 'NONE', #499, 10.00000000000000178 ) ;
#722 = CARTESIAN_POINT ( 'NONE',  ( 3.556430356250014579, 108.1539533981018053, 3.865625000614517415 ) ) ;
#723 = PRODUCT_DEFINITION_SHAPE ( 'NONE', 'NONE',  #12956 ) ;
#724 = ORIENTED_EDGE ( 'NONE', *, *, #4951, .F. ) ;
#725 = EDGE_CURVE ( 'NONE', #12624, #3688, #9320, .T. ) ;
#726 = AXIS2_PLACEMENT_3D ( 'NONE', #602, #12590, #3632 ) ;
#727 = CARTESIAN_POINT ( 'NONE',  ( -60.00000000000000000, 30.00000000000000000, 9.999999999999996447 ) ) ;
#728 = DIRECTION ( 'NONE',  ( 0.000000000000000000, -1.000000000000000000, 0.000000000000000000 ) ) ;
#729 = FILL_AREA_STYLE_COLOUR ( '', #2356 ) ;
#730 = CARTESIAN_POINT ( 'NONE',  ( 66.19999999999998863, 90.00000000000000000, 4.437500001229033764 ) ) ;
#731 = EDGE_CURVE ( 'NONE', #10645, #11257, #10099, .T. ) ;
#732 = CIRCLE ( 'NONE', #5327, 1.499999999999999556 ) ;
#733 = CARTESIAN_POINT ( 'NONE',  ( -61.00000000000000711, 26.13129029178200469, 0.9999999999999926725 ) ) ;
#734 = CIRCLE ( 'NONE', #6785, 1.599999999999997202 ) ;
#735 = CARTESIAN_POINT ( 'NONE',  ( 66.19999999999997442, 108.0133283987163253, 4.812500000000000000 ) ) ;
#736 = CARTESIAN_POINT ( 'NONE',  ( 35.75000000000000711, 92.49999999999998579, -4.802775637732004554 ) ) ;
#737 = DIRECTION ( 'NONE',  ( -0.000000000000000000, -0.000000000000000000, -1.000000000000000000 ) ) ;
#738 = CARTESIAN_POINT ( 'NONE',  ( 31.50000000000000000, 90.00000000000000000, -8.000000000000000000 ) ) ;
#739 = EDGE_CURVE ( 'NONE', #5916, #6728, #5927, .T. ) ;
#740 = CARTESIAN_POINT ( 'NONE',  ( 1.617350269189632428, 0.000000000000000000, 0.000000000000000000 ) ) ;
#741 = CARTESIAN_POINT ( 'NONE',  ( 19.27821517812500574, 117.2309300971526937, 3.884375000614516793 ) ) ;
#742 = ORIENTED_EDGE ( 'NONE', *, *, #6361, .T. ) ;
#743 = CIRCLE ( 'NONE', #2637, 1.500000000000001332 ) ;
#744 = CARTESIAN_POINT ( 'NONE',  ( 66.20000000000000284, 71.98667160128370313, 4.287500000000000533 ) ) ;
#745 = DIRECTION ( 'NONE',  ( 1.000000000000000000, 1.281026566875180806E-14, 0.000000000000000000 ) ) ;
#746 = ORIENTED_EDGE ( 'NONE', *, *, #952, .T. ) ;
#747 = EDGE_CURVE ( 'NONE', #10649, #11707, #5061, .T. ) ;
#748 = DIRECTION ( 'NONE',  ( 0.000000000000000000, 0.000000000000000000, -1.000000000000000000 ) ) ;
#749 = CARTESIAN_POINT ( 'NONE',  ( 5.000000000000007994, 90.00000000000000000, -3.000000000000000000 ) ) ;
#750 = VECTOR ( 'NONE', #11166, 1000.000000000000000 ) ;
#751 = CARTESIAN_POINT ( 'NONE',  ( 5.000000000000004441, 30.00000000000000000, -2.500000000000000444 ) ) ;
#752 = CARTESIAN_POINT ( 'NONE',  ( 3.556430356250014579, 108.1539533981018053, 3.415625000614516793 ) ) ;
#753 = DIRECTION ( 'NONE',  ( 1.000000000000000000, 0.000000000000000000, 0.000000000000000000 ) ) ;
#754 = CARTESIAN_POINT ( 'NONE',  ( 3.556430356250015024, 90.00000000000000000, 4.859375000614517326 ) ) ;
#755 = EDGE_LOOP ( 'NONE', ( #10469, #5474, #7145, #11199 ) ) ;
#756 = EDGE_CURVE ( 'NONE', #5282, #3511, #6243, .T. ) ;
#757 = CARTESIAN_POINT ( 'NONE',  ( 3.800000000000001155, 108.0133283987163111, 4.512500000000001066 ) ) ;
#758 = ORIENTED_EDGE ( 'NONE', *, *, #6666, .T. ) ;
#759 = ADVANCED_FACE ( 'NONE', ( #3115 ), #7095, .F. ) ;
#760 = CIRCLE ( 'NONE', #2246, 1.500000000000001332 ) ;
#761 =( LENGTH_UNIT ( ) NAMED_UNIT ( * ) SI_UNIT ( .MILLI., .METRE. ) );
#762 = DIRECTION ( 'NONE',  ( -0.000000000000000000, -1.000000000000000000, -0.000000000000000000 ) ) ;
#763 = CARTESIAN_POINT ( 'NONE',  ( 19.40000000000000924, 117.0199925980744666, 4.474999999999999645 ) ) ;
#764 = DIRECTION ( 'NONE',  ( -1.000000000000000000, 0.000000000000000000, 0.000000000000000000 ) ) ;
#765 = ORIENTED_EDGE ( 'NONE', *, *, #4326, .T. ) ;
#766 = PLANE ( 'NONE',  #12339 ) ;
#767 = VERTEX_POINT ( 'NONE', #5128 ) ;
#768 = LINE ( 'NONE', #8696, #9080 ) ;
#769 = CARTESIAN_POINT ( 'NONE',  ( 34.25000000000000000, 92.49999999999998579, 4.000000000000000000 ) ) ;
#770 = CIRCLE ( 'NONE', #12057, 1.599999999999997202 ) ;
#771 = ORIENTED_EDGE ( 'NONE', *, *, #10941, .T. ) ;
#772 = CARTESIAN_POINT ( 'NONE',  ( 28.99095782554748624, 92.47818727009294548, 4.000000000000000000 ) ) ;
#773 = ORIENTED_EDGE ( 'NONE', *, *, #1233, .T. ) ;
#774 = ADVANCED_FACE ( 'NONE', ( #8212, #1329 ), #3249, .F. ) ;
#775 = ORIENTED_EDGE ( 'NONE', *, *, #2311, .F. ) ;
#776 = DIRECTION ( 'NONE',  ( -1.000000000000000000, 0.000000000000000000, 0.000000000000000000 ) ) ;
#777 = DIRECTION ( 'NONE',  ( 0.4719909656437444867, -0.8816033849473842166, 0.000000000000000000 ) ) ;
#778 = VECTOR ( 'NONE', #11676, 1000.000000000000000 ) ;
#779 = ORIENTED_EDGE ( 'NONE', *, *, #2404, .T. ) ;
#780 = CARTESIAN_POINT ( 'NONE',  ( 4.763019983628629994, -4.349268977144817860, 0.000000000000000000 ) ) ;
#781 = ORIENTED_EDGE ( 'NONE', *, *, #10591, .T. ) ;
#782 = ORIENTED_EDGE ( 'NONE', *, *, #419, .T. ) ;
#783 = CARTESIAN_POINT ( 'NONE',  ( 64.54728994471078352, 100.7543353520590870, 2.802601390178781404 ) ) ;
#784 = ORIENTED_EDGE ( 'NONE', *, *, #3580, .T. ) ;
#785 = CIRCLE ( 'NONE', #2474, 3.500000000000003109 ) ;
#786 = CARTESIAN_POINT ( 'NONE',  ( 30.00000000000000711, 0.000000000000000000, -10.00000000000000000 ) ) ;
#787 = DIRECTION ( 'NONE',  ( -1.000000000000000000, 0.000000000000000000, 0.000000000000000000 ) ) ;
#788 = DIRECTION ( 'NONE',  ( -0.000000000000000000, 1.000000000000000000, -0.000000000000000000 ) ) ;
#789 = CARTESIAN_POINT ( 'NONE',  ( 35.00000000000000000, 126.0266567974326222, 4.550000001229034474 ) ) ;
#790 = DIRECTION ( 'NONE',  ( -1.084202172485503571E-16, 0.000000000000000000, 1.000000000000000000 ) ) ;
#791 = EDGE_CURVE ( 'NONE', #9339, #7595, #7229, .T. ) ;
#792 = CIRCLE ( 'NONE', #10416, 1.599999999999992095 ) ;
#794 = EDGE_CURVE ( 'NONE', #11167, #1351, #9250, .T. ) ;
#793 = CARTESIAN_POINT ( 'NONE',  ( -57.99999999999999289, 30.00000000000000000, -8.000000000000003553 ) ) ;
#795 = CARTESIAN_POINT ( 'NONE',  ( 64.24207199149496716, 100.8784753363798075, 2.999999999999999556 ) ) ;
#796 = DIRECTION ( 'NONE',  ( -0.3262398754384820410, 0.9452870165584015272, 0.000000000000000000 ) ) ;
#797 = DIRECTION ( 'NONE',  ( 0.000000000000000000, 0.000000000000000000, 1.000000000000000000 ) ) ;
#798 =( BOUNDED_CURVE ( )  B_SPLINE_CURVE ( 2, ( #1403, #9385, #542, #2657, #11475, #10628, #6566 ),
 .UNSPECIFIED., .F., .F. ) 
 B_SPLINE_CURVE_WITH_KNOTS ( ( 3, 2, 2, 3 ),
 ( 0.3999999999999999667, 0.4333333333333333481, 0.4666666666666667296, 0.5000000000000001110 ),
 .UNSPECIFIED. ) 
 CURVE ( )  GEOMETRIC_REPRESENTATION_ITEM ( )  RATIONAL_B_SPLINE_CURVE ( ( 1.000000000000000444, 0.8660254037844385966, 1.000000000000000000, 0.8660254037844387076, 1.000000000000000000, 0.8660254037844382635, 1.000000000000000444 ) ) 
 REPRESENTATION_ITEM ( '' )  );
#799 = DIRECTION ( 'NONE',  ( 0.000000000000000000, 0.000000000000000000, 1.000000000000000000 ) ) ;
#800 = FACE_OUTER_BOUND ( 'NONE', #9608, .T. ) ;
#801 = CARTESIAN_POINT ( 'NONE',  ( 3.556430356250015024, 90.00000000000000000, 4.859375000614517326 ) ) ;
#802 = ORIENTED_EDGE ( 'NONE', *, *, #7272, .F. ) ;
#803 = CIRCLE ( 'NONE', #8129, 1.500000000000003331 ) ;
#804 = CARTESIAN_POINT ( 'NONE',  ( 50.59999999999999432, 117.0199925980744666, 4.850000000000000533 ) ) ;
#805 = PLANE ( 'NONE',  #2672 ) ;
#806 = ORIENTED_EDGE ( 'NONE', *, *, #5628, .F. ) ;
#807 = VECTOR ( 'NONE', #5449, 1000.000000000000000 ) ;
#808 = DIRECTION ( 'NONE',  ( -0.000000000000000000, -0.000000000000000000, -1.000000000000000000 ) ) ;
#809 = FACE_OUTER_BOUND ( 'NONE', #2682, .T. ) ;
#810 = VECTOR ( 'NONE', #8844, 1000.000000000000000 ) ;
#811 = LINE ( 'NONE', #3838, #1160 ) ;
#812 = EDGE_CURVE ( 'NONE', #6247, #5477, #281, .T. ) ;
#813 = CARTESIAN_POINT ( 'NONE',  ( 35.00000000000000000, 126.3079067962036106, 4.240625000614517859 ) ) ;
#814 = CARTESIAN_POINT ( 'NONE',  ( 28.68194083117252902, 91.52713075379780605, -0.9999999999999970024 ) ) ;
#815 = CARTESIAN_POINT ( 'NONE',  ( 19.27821517812500574, 117.2309300971526937, 3.884375000614516793 ) ) ;
#816 = ORIENTED_EDGE ( 'NONE', *, *, #3757, .T. ) ;
#817 = CIRCLE ( 'NONE', #12527, 2.396199811936269963 ) ;
#818 = CARTESIAN_POINT ( 'NONE',  ( 9.650000000000000355, 0.000000000000000000, 0.000000000000000000 ) ) ;
#819 = EDGE_LOOP ( 'NONE', ( #12547, #8502, #7527, #504 ) ) ;
#820 = PLANE ( 'NONE',  #10704 ) ;
#821 = CARTESIAN_POINT ( 'NONE',  ( 35.00000000000000000, 90.00000000000000000, 5.000000000000000000 ) ) ;
#822 = DIRECTION ( 'NONE',  ( -0.000000000000000000, -0.000000000000000000, 1.000000000000000000 ) ) ;
#824 = ADVANCED_FACE ( 'NONE', ( #3571 ), #6132, .F. ) ;
#823 = DIRECTION ( 'NONE',  ( -0.000000000000000000, 0.000000000000000000, 1.000000000000000000 ) ) ;
#825 = PRODUCT_DEFINITION_SHAPE ( 'NONE', 'NONE',  #12957 ) ;
#826 = DIRECTION ( 'NONE',  ( 0.5000000000000005551, -0.8660254037844383745, 0.000000000000000000 ) ) ;
#828 = CARTESIAN_POINT ( 'NONE',  ( 35.49999999999995026, 119.0000000000000000, 4.000000000000000000 ) ) ;
#827 = CIRCLE ( 'NONE', #4601, 1.500000000000001332 ) ;
#829 = ORIENTED_EDGE ( 'NONE', *, *, #3040, .F. ) ;
#830 = CARTESIAN_POINT ( 'NONE',  ( -0.1325741768533960641, -4.273461295629625845, 0.000000000000000000 ) ) ;
#831 = EDGE_CURVE ( 'NONE', #10785, #11574, #3505, .T. ) ;
#832 = ITEM_DEFINED_TRANSFORMATION ( 'NONE', 'NONE', #11145,  #5704 ) ;
#833 = DIRECTION ( 'NONE',  ( -1.000000000000000000, -0.000000000000000000, -0.000000000000000000 ) ) ;
#834 = EDGE_LOOP ( 'NONE', ( #3807, #9213, #11904 ) ) ;
#835 = VERTEX_POINT ( 'NONE', #7421 ) ;
#836 = CYLINDRICAL_SURFACE ( 'NONE', #9008, 1.500000000000001332 ) ;
#837 = ORIENTED_EDGE ( 'NONE', *, *, #6720, .T. ) ;
#838 = DIRECTION ( 'NONE',  ( -1.000000000000000000, 0.000000000000000000, 0.000000000000000000 ) ) ;
#839 = AXIS2_PLACEMENT_3D ( 'NONE', #8214, #8409, #1467 ) ;
#840 = CARTESIAN_POINT ( 'NONE',  ( 19.89999999999999503, 90.00000000000000000, -10.00000000000000000 ) ) ;
#841 = EDGE_CURVE ( 'NONE', #3363, #7515, #10366, .T. ) ;
#842 = ORIENTED_EDGE ( 'NONE', *, *, #4723, .T. ) ;
#843 = LINE ( 'NONE', #2699, #6376 ) ;
#844 = ORIENTED_EDGE ( 'NONE', *, *, #11090, .F. ) ;
#845 = DIRECTION ( 'NONE',  ( 0.000000000000000000, 0.000000000000000000, 1.000000000000000000 ) ) ;
#846 = EDGE_LOOP ( 'NONE', ( #6406, #7183, #10691, #3671 ) ) ;
#847 = VECTOR ( 'NONE', #8727, 1000.000000000000000 ) ;
#848 = CARTESIAN_POINT ( 'NONE',  ( 0.000000000000000000, 2.000000000000000000, 0.000000000000000000 ) ) ;
#849 = ORIENTED_EDGE ( 'NONE', *, *, #1595, .F. ) ;
#850 = CARTESIAN_POINT ( 'NONE',  ( 1.750000000000000000, 0.000000000000000000, 1.499999999999999556 ) ) ;
#851 = CARTESIAN_POINT ( 'NONE',  ( 34.25000000000000000, 93.41869858279433458, -3.000000000000000000 ) ) ;
#852 = CARTESIAN_POINT ( 'NONE',  ( 35.00000000000000000, 126.3079067962035822, 3.340625000614517059 ) ) ;
#853 = AXIS2_PLACEMENT_3D ( 'NONE', #3691, #4729, #3625 ) ;
#854 = CARTESIAN_POINT ( 'NONE',  ( -998.3826497308103853, 0.000000000000000000, 0.000000000000000000 ) ) ;
#855 = ADVANCED_FACE ( 'NONE', ( #4477 ), #5384, .F. ) ;
#856 = CARTESIAN_POINT ( 'NONE',  ( 3.800000000000015365, 90.00000000000000000, 4.549999999999999822 ) ) ;
#857 = DIRECTION ( 'NONE',  ( -0.000000000000000000, -0.000000000000000000, -1.000000000000000000 ) ) ;
#858 = CARTESIAN_POINT ( 'NONE',  ( 51.63879093662676922, 66.24814457421848601, 2.000000000000002220 ) ) ;
#859 = CARTESIAN_POINT ( 'NONE',  ( 1.040000000000000036, -0.5773502691896256200, -1.000000000000000000 ) ) ;
#860 = LINE ( 'NONE', #11926, #9943 ) ;
#861 = EDGE_LOOP ( 'NONE', ( #5404, #2432, #3556, #8105 ) ) ;
#862 = VECTOR ( 'NONE', #12886, 1000.000000000000000 ) ;
#863 = PLANE ( 'NONE',  #9839 ) ;
#864 = CARTESIAN_POINT ( 'NONE',  ( 35.00000000000000711, 53.69209320379640360, 4.071875000614516793 ) ) ;
#866 = ADVANCED_FACE ( 'NONE', ( #2390 ), #7550, .T. ) ;
#865 = VERTEX_POINT ( 'NONE', #12592 ) ;
#867 = EDGE_CURVE ( 'NONE', #12412, #10917, #6497, .T. ) ;
#868 = CARTESIAN_POINT ( 'NONE',  ( 50.60000000000001563, 62.98000740192552627, 3.350000000000000533 ) ) ;
#869 = LINE ( 'NONE', #9776, #11647 ) ;
#870 = VERTEX_POINT ( 'NONE', #2582 ) ;
#871 = AXIS2_PLACEMENT_3D ( 'NONE', #9762, #2644, #10806 ) ;
#872 = CYLINDRICAL_SURFACE ( 'NONE', #11788, 1.499999999999999556 ) ;
#873 = ADVANCED_FACE ( 'NONE', ( #1662 ), #6562, .F. ) ;
#874 = DIRECTION ( 'NONE',  ( -1.000000000000000000, -0.000000000000000000, -0.000000000000000000 ) ) ;
#875 = DIRECTION ( 'NONE',  ( 1.000000000000000000, 0.000000000000000000, 0.000000000000000000 ) ) ;
#876 = CARTESIAN_POINT ( 'NONE',  ( -38.66666666666665719, 30.00000000000000000, -7.999999999999996447 ) ) ;
#877 = CARTESIAN_POINT ( 'NONE',  ( 19.27821517812500574, 117.2309300971526937, 4.334375000614516971 ) ) ;
#878 = ORIENTED_EDGE ( 'NONE', *, *, #10870, .F. ) ;
#879 = AXIS2_PLACEMENT_3D ( 'NONE', #12949, #12888, #6862 ) ;
#880 = CARTESIAN_POINT ( 'NONE',  ( 60.00000000000000000, 0.000000000000000000, 15.00000000000000000 ) ) ;
#881 = ORIENTED_EDGE ( 'NONE', *, *, #2430, .T. ) ;
#882 =( NAMED_UNIT ( * ) SI_UNIT ( $, .STERADIAN. ) SOLID_ANGLE_UNIT ( ) );
#883 = ADVANCED_FACE ( 'NONE', ( #10491 ), #5650, .F. ) ;
#884 = LINE ( 'NONE', #4888, #12292 ) ;
#885 = CARTESIAN_POINT ( 'NONE',  ( 21.49999999999998579, 90.00000000000000000, -10.00000000000000000 ) ) ;
#886 = CARTESIAN_POINT ( 'NONE',  ( -60.00000000000000000, -6.000000000000000000, 14.99999999999999645 ) ) ;
#887 = DIRECTION ( 'NONE',  ( -0.000000000000000000, 0.000000000000000000, 1.000000000000000000 ) ) ;
#888 = ORIENTED_EDGE ( 'NONE', *, *, #8720, .T. ) ;
#889 = DIRECTION ( 'NONE',  ( 0.3090169943749451753, 0.9510565162951544194, -0.000000000000000000 ) ) ;
#890 = CARTESIAN_POINT ( 'NONE',  ( 66.19999999999998863, 90.00000000000000000, 5.000000000000000000 ) ) ;
#891 = ORIENTED_EDGE ( 'NONE', *, *, #5454, .T. ) ;
#892 = VECTOR ( 'NONE', #11066, 1000.000000000000000 ) ;
#893 = FACE_OUTER_BOUND ( 'NONE', #5421, .T. ) ;
#894 = ORIENTED_EDGE ( 'NONE', *, *, #6652, .T. ) ;
#895 = EDGE_CURVE ( 'NONE', #11453, #7103, #8540, .T. ) ;
#896 = ORIENTED_EDGE ( 'NONE', *, *, #10776, .T. ) ;
#897 = CARTESIAN_POINT ( 'NONE',  ( 50.00000000000000000, 62.64236852357281293, 1.500000000000001332 ) ) ;
#898 =( GEOMETRIC_REPRESENTATION_CONTEXT ( 3 ) GLOBAL_UNCERTAINTY_ASSIGNED_CONTEXT ( ( #6165 ) ) GLOBAL_UNIT_ASSIGNED_CONTEXT ( ( #7994, #6701, #11056 ) ) REPRESENTATION_CONTEXT ( 'NONE', 'WORKASPACE' ) );
#899 = PLANE ( 'NONE',  #11027 ) ;
#900 = ADVANCED_FACE ( 'NONE', ( #10563 ), #6369, .F. ) ;
#901 = ORIENTED_EDGE ( 'NONE', *, *, #7854, .T. ) ;
#902 = PLANE ( 'NONE',  #6579 ) ;
#903 = ORIENTED_EDGE ( 'NONE', *, *, #10354, .F. ) ;
#904 = APPLICATION_CONTEXT ( 'automotive_design' ) ;
#905 = CARTESIAN_POINT ( 'NONE',  ( 35.00000000000000000, 90.00000000000000000, -1.000000000000000000 ) ) ;
#906 = CARTESIAN_POINT ( 'NONE',  ( 39.63969097257307794, 121.0132401377472036, 3.000000000000001776 ) ) ;
#907 = ORIENTED_EDGE ( 'NONE', *, *, #8637, .T. ) ;
#908 = CARTESIAN_POINT ( 'NONE',  ( 19.27821517812503060, 62.76906990284727783, 4.428125000614516971 ) ) ;
#909 = ORIENTED_EDGE ( 'NONE', *, *, #6026, .T. ) ;
#910 = FACE_OUTER_BOUND ( 'NONE', #4176, .T. ) ;
#911 = AXIS2_PLACEMENT_3D ( 'NONE', #416, #4429, #5462 ) ;
#912 = LINE ( 'NONE', #11787, #8517 ) ;
#913 = EDGE_CURVE ( 'NONE', #11775, #4019, #4893, .T. ) ;
#914 = VECTOR ( 'NONE', #1674, 1000.000000000000000 ) ;
#915 = FACE_OUTER_BOUND ( 'NONE', #12172, .T. ) ;
#916 = CARTESIAN_POINT ( 'NONE',  ( 19.27821517812503060, 62.76906990284727783, 3.978125000614516793 ) ) ;
#917 = EDGE_CURVE ( 'NONE', #12608, #8631, #537, .T. ) ;
#918 = FACE_OUTER_BOUND ( 'NONE', #4746, .T. ) ;
#919 = VERTEX_POINT ( 'NONE', #604 ) ;
#920 = DIRECTION ( 'NONE',  ( -1.000000000000000000, 0.000000000000000000, 0.000000000000000000 ) ) ;
#921 = AXIS2_PLACEMENT_3D ( 'NONE', #2490, #6466, #10462 ) ;
#922 = LINE ( 'NONE', #11728, #1022 ) ;
#923 = LINE ( 'NONE', #4988, #10114 ) ;
#924 = ORIENTED_EDGE ( 'NONE', *, *, #8530, .F. ) ;
#925 = CIRCLE ( 'NONE', #9082, 32.70000000000000995 ) ;
#926 = CARTESIAN_POINT ( 'NONE',  ( -998.3826497308103853, 0.000000000000000000, 0.000000000000000000 ) ) ;
#927 = ORIENTED_EDGE ( 'NONE', *, *, #11531, .F. ) ;
#928 = PLANE ( 'NONE',  #5027 ) ;
#929 = CARTESIAN_POINT ( 'NONE',  ( 35.00000000000000711, 53.69209320379640360, 3.171875000614517326 ) ) ;
#930 = ORIENTED_EDGE ( 'NONE', *, *, #4986, .T. ) ;
#931 = EDGE_CURVE ( 'NONE', #1668, #8414, #9445, .T. ) ;
#932 = CARTESIAN_POINT ( 'NONE',  ( 19.27821517812500574, 117.2309300971526937, 4.784375000614516260 ) ) ;
#933 = DIRECTION ( 'NONE',  ( -0.000000000000000000, -0.000000000000000000, -1.000000000000000000 ) ) ;
#934 = AXIS2_PLACEMENT_3D ( 'NONE', #10445, #11553, #3520 ) ;
#935 = AXIS2_PLACEMENT_3D ( 'NONE', #9020, #5227, #4059 ) ;
#936 = FILL_AREA_STYLE ('',( #9905 ) ) ;
#937 = DIRECTION ( 'NONE',  ( 0.000000000000000000, 0.000000000000000000, 1.000000000000000000 ) ) ;
#938 = EDGE_CURVE ( 'NONE', #252, #6072, #5110, .T. ) ;
#939 = VECTOR ( 'NONE', #10169, 1000.000000000000000 ) ;
#940 = CARTESIAN_POINT ( 'NONE',  ( 35.00000000000000000, 90.00000000000000000, -1.000000000000000888 ) ) ;
#941 = AXIS2_PLACEMENT_3D ( 'NONE', #12279, #5334, #12079 ) ;
#942 = CARTESIAN_POINT ( 'NONE',  ( 39.21379230364324542, 85.05086326499692007, 22.38477631085024555 ) ) ;
#943 = DIRECTION ( 'NONE',  ( -0.000000000000000000, 0.000000000000000000, -1.000000000000000000 ) ) ;
#944 = ORIENTED_EDGE ( 'NONE', *, *, #9425, .F. ) ;
#945 = CARTESIAN_POINT ( 'NONE',  ( 1.269999999999999796, 3.490243377569955568E-16, -2.849999999999999201 ) ) ;
#946 = VERTEX_POINT ( 'NONE', #11338 ) ;
#947 = SURFACE_SIDE_STYLE ('',( #20 ) ) ;
#948 = AXIS2_PLACEMENT_3D ( 'NONE', #2780, #4020, #9961 ) ;
#949 = COLOUR_RGB ( '',0.8941176470588234615, 0.8941176470588234615, 0.8941176470588234615 ) ;
#950 = DIRECTION ( 'NONE',  ( 0.000000000000000000, 0.000000000000000000, 1.000000000000000000 ) ) ;
#951 = DIRECTION ( 'NONE',  ( 1.301042606982605124E-15, 7.511572993685881931E-16, 1.000000000000000000 ) ) ;
#952 = EDGE_CURVE ( 'NONE', #10652, #7727, #7415, .T. ) ;
#953 = DIRECTION ( 'NONE',  ( 1.000000000000000000, 0.000000000000000000, 0.000000000000000000 ) ) ;
#954 = ADVANCED_FACE ( 'NONE', ( #9768 ), #6949, .T. ) ;
#955 = VERTEX_POINT ( 'NONE', #7679 ) ;
#956 = DIRECTION ( 'NONE',  ( -0.000000000000000000, 1.000000000000000000, -0.000000000000000000 ) ) ;
#957 = ITEM_DEFINED_TRANSFORMATION ( 'NONE', 'NONE', #2804,  #5704 ) ;
#958 = DIRECTION ( 'NONE',  ( 0.000000000000000000, 0.000000000000000000, 1.000000000000000000 ) ) ;
#959 = ORIENTED_EDGE ( 'NONE', *, *, #12861, .F. ) ;
#960 = FILL_AREA_STYLE_COLOUR ( '', #10521 ) ;
#961 = DIRECTION ( 'NONE',  ( -0.000000000000000000, 1.000000000000000000, -0.000000000000000000 ) ) ;
#962 = ORIENTED_EDGE ( 'NONE', *, *, #8949, .F. ) ;
#963 = VECTOR ( 'NONE', #2574, 1000.000000000000000 ) ;
#964 = CARTESIAN_POINT ( 'NONE',  ( 25.00000000000000355, 0.000000000000000000, 5.750000000000000000 ) ) ;
#965 = ORIENTED_EDGE ( 'NONE', *, *, #11531, .T. ) ;
#966 = CARTESIAN_POINT ( 'NONE',  ( 36.50000000000001421, 67.79999999999999716, 6.000000000000000000 ) ) ;
#967 = DIRECTION ( 'NONE',  ( 0.000000000000000000, 0.000000000000000000, -1.000000000000000000 ) ) ;
#968 = ORIENTED_EDGE ( 'NONE', *, *, #12311, .F. ) ;
#969 = ORIENTED_EDGE ( 'NONE', *, *, #12016, .T. ) ;
#970 = CIRCLE ( 'NONE', #10176, 28.99999999999999289 ) ;
#971 = DIRECTION ( 'NONE',  ( -0.000000000000000000, -0.000000000000000000, -1.000000000000000000 ) ) ;
#972 = EDGE_LOOP ( 'NONE', ( #6350, #4719, #5970 ) ) ;
#973 = DIRECTION ( 'NONE',  ( 0.000000000000000000, 0.000000000000000000, 1.000000000000000000 ) ) ;
#974 = ORIENTED_EDGE ( 'NONE', *, *, #4443, .F. ) ;
#975 = CARTESIAN_POINT ( 'NONE',  ( 66.44356964374999563, 71.84604660189820891, 4.090625000614517504 ) ) ;
#976 = EDGE_CURVE ( 'NONE', #11967, #1106, #7871, .T. ) ;
#977 = VERTEX_POINT ( 'NONE', #2845 ) ;
#978 = CARTESIAN_POINT ( 'NONE',  ( 9.999999999999994671, 70.41451884327426569, -2.500000000000000000 ) ) ;
#979 = CARTESIAN_POINT ( 'NONE',  ( 3.556430356250014579, 108.1539533981018053, 4.765625000614517326 ) ) ;
#980 = CIRCLE ( 'NONE', #9970, 4.000000000000000000 ) ;
#981 = DIRECTION ( 'NONE',  ( -0.000000000000000000, -0.000000000000000000, 1.000000000000000000 ) ) ;
#982 = CARTESIAN_POINT ( 'NONE',  ( 66.44356964374999563, 90.00000000000000000, 4.128125000614517148 ) ) ;
#983 = DIRECTION ( 'NONE',  ( -0.000000000000000000, 0.000000000000000000, 1.000000000000000000 ) ) ;
#984 = ORIENTED_EDGE ( 'NONE', *, *, #7294, .F. ) ;
#985 = SHAPE_REPRESENTATION ( 'buckets', ( #5704 ), #1096 ) ;
#986 = DIRECTION ( 'NONE',  ( 1.000000000000000000, -0.000000000000000000, -0.000000000000000000 ) ) ;
#987 = EDGE_CURVE ( 'NONE', #10383, #11518, #2907, .T. ) ;
#988 = EDGE_CURVE ( 'NONE', #4325, #9537, #6991, .T. ) ;
#989 = FACE_OUTER_BOUND ( 'NONE', #12469, .T. ) ;
#990 = DIRECTION ( 'NONE',  ( -0.000000000000000000, -0.000000000000000000, -1.000000000000000000 ) ) ;
#991 = AXIS2_PLACEMENT_3D ( 'NONE', #6237, #12192, #2261 ) ;
#992 = VERTEX_POINT ( 'NONE', #5842 ) ;
#993 = DIRECTION ( 'NONE',  ( 1.000000000000000000, 0.000000000000000000, 0.000000000000000000 ) ) ;
#994 = EDGE_CURVE ( 'NONE', #5904, #1184, #923, .T. ) ;
#995 = EDGE_LOOP ( 'NONE', ( #11036, #8835, #1603, #7933 ) ) ;
#996 = DIRECTION ( 'NONE',  ( -0.000000000000000000, -0.000000000000000000, -1.000000000000000000 ) ) ;
#997 = CARTESIAN_POINT ( 'NONE',  ( 3.556430356250014579, 108.1539533981018053, 4.765625000614517326 ) ) ;
#998 = VERTEX_POINT ( 'NONE', #7937 ) ;
#999 = CARTESIAN_POINT ( 'NONE',  ( 60.63303221600038739, 111.5086687461494392, 2.885734441893565538 ) ) ;
#1000 = CARTESIAN_POINT ( 'NONE',  ( 4.270088556250601699E-16, 30.00000000000000000, -8.000000000000000000 ) ) ;
#1001 = CIRCLE ( 'NONE', #4975, 1.599999999999997202 ) ;
#1002 = CIRCLE ( 'NONE', #8121, 28.99999999999999289 ) ;
#1003 = CARTESIAN_POINT ( 'NONE',  ( -43.33333333333332860, 79.07477288111861924, 0.9999999999999997780 ) ) ;
#1004 = EDGE_CURVE ( 'NONE', #6272, #8022, #6754, .T. ) ;
#1005 = LINE ( 'NONE', #10886, #10745 ) ;
#1006 = CARTESIAN_POINT ( 'NONE',  ( 64.47099661891826372, 100.7265662098818098, 2.905726390019228056 ) ) ;
#1007 = DIRECTION ( 'NONE',  ( -0.000000000000000000, 0.000000000000000000, 1.000000000000000000 ) ) ;
#1008 = DIRECTION ( 'NONE',  ( -1.000000000000000000, 0.000000000000000000, 0.000000000000000000 ) ) ;
#1009 = ORIENTED_EDGE ( 'NONE', *, *, #10776, .F. ) ;
#1010 = CARTESIAN_POINT ( 'NONE',  ( 0.1325741768533959530, -4.273461295629625845, -0.8000000000000000444 ) ) ;
#1011 = ORIENTED_EDGE ( 'NONE', *, *, #12514, .F. ) ;
#1012 = AXIS2_PLACEMENT_3D ( 'NONE', #9319, #2389, #5259 ) ;
#1013 = VECTOR ( 'NONE', #9574, 1000.000000000000000 ) ;
#1014 = CARTESIAN_POINT ( 'NONE',  ( 3.800000000000015810, 108.0133283987162969, 3.612500000000000711 ) ) ;
#1015 = CARTESIAN_POINT ( 'NONE',  ( 20.00000000000000355, 0.000000000000000000, -10.00000000000000000 ) ) ;
#1016 = EDGE_CURVE ( 'NONE', #11762, #12580, #2408, .T. ) ;
#1017 = CARTESIAN_POINT ( 'NONE',  ( 1.040000000000000036, 0.000000000000000000, 0.000000000000000000 ) ) ;
#1018 = VERTEX_POINT ( 'NONE', #1792 ) ;
#1019 = DIRECTION ( 'NONE',  ( 0.000000000000000000, 0.000000000000000000, -1.000000000000000000 ) ) ;
#1020 = DIRECTION ( 'NONE',  ( 0.000000000000000000, 0.000000000000000000, 1.000000000000000000 ) ) ;
#1021 = ORIENTED_EDGE ( 'NONE', *, *, #1157, .F. ) ;
#1022 = VECTOR ( 'NONE', #6753, 1000.000000000000000 ) ;
#1023 = EDGE_CURVE ( 'NONE', #9939, #1488, #2969, .T. ) ;
#1024 = SURFACE_SIDE_STYLE ('',( #11096 ) ) ;
#1025 = PRESENTATION_STYLE_ASSIGNMENT (( #5933 ) ) ;
#1026 = ORIENTED_EDGE ( 'NONE', *, *, #5667, .T. ) ;
#1027 = DIRECTION ( 'NONE',  ( -1.000000000000000000, 0.000000000000000000, 1.084202172485504064E-16 ) ) ;
#1028 = ORIENTED_EDGE ( 'NONE', *, *, #8827, .F. ) ;
#1029 = EDGE_CURVE ( 'NONE', #1627, #698, #2822, .T. ) ;
#1030 = EDGE_CURVE ( 'NONE', #9167, #11004, #12112, .T. ) ;
#1031 = FACE_OUTER_BOUND ( 'NONE', #3643, .T. ) ;
#1032 = CARTESIAN_POINT ( 'NONE',  ( 3.000000000000004441, 30.00000000000000000, -10.00000000000000000 ) ) ;
#1033 = ORIENTED_EDGE ( 'NONE', *, *, #2858, .T. ) ;
#1034 = VECTOR ( 'NONE', #3985, 1000.000000000000000 ) ;
#1035 = ORIENTED_EDGE ( 'NONE', *, *, #1030, .F. ) ;
#1036 = CARTESIAN_POINT ( 'NONE',  ( 35.00000000000000000, 90.00000000000000000, -8.000000000000000000 ) ) ;
#1037 = ORIENTED_EDGE ( 'NONE', *, *, #2209, .F. ) ;
#1038 = CARTESIAN_POINT ( 'NONE',  ( 66.44356964374999563, 71.84604660189820891, 4.540625000614517681 ) ) ;
#1039 = ORIENTED_EDGE ( 'NONE', *, *, #1444, .F. ) ;
#1040 = DIRECTION ( 'NONE',  ( -1.000000000000000000, -0.000000000000000000, -0.000000000000000000 ) ) ;
#1041 = EDGE_LOOP ( 'NONE', ( #5551, #7064, #7845, #6591 ) ) ;
#1042 = VECTOR ( 'NONE', #2332, 1000.000000000000000 ) ;
#1043 = CARTESIAN_POINT ( 'NONE',  ( 17.49999999999998579, 90.00000000000002842, -8.000000000000000000 ) ) ;
#1044 = CIRCLE ( 'NONE', #2106, 1.599999999999998757 ) ;
#1045 = CARTESIAN_POINT ( 'NONE',  ( 3.591865698314129496, 91.49237114305354623, 2.999999999999999556 ) ) ;
#1046 = DIRECTION ( 'NONE',  ( -0.000000000000000000, 1.000000000000000000, -0.000000000000000000 ) ) ;
#1047 = CARTESIAN_POINT ( 'NONE',  ( 34.49999999999995026, 119.0000000000000000, 4.000000000000000000 ) ) ;
#1048 = DIRECTION ( 'NONE',  ( -1.000000000000000000, 0.000000000000000000, -5.337610695313252124E-17 ) ) ;
#1049 = EDGE_CURVE ( 'NONE', #58, #8179, #6691, .T. ) ;
#1050 = VERTEX_POINT ( 'NONE', #4863 ) ;
#1051 = AXIS2_PLACEMENT_3D ( 'NONE', #10287, #5252, #6234 ) ;
#1052 = CARTESIAN_POINT ( 'NONE',  ( 66.19999999999998863, 90.00000000000000000, 4.774999999999999467 ) ) ;
#1053 = LINE ( 'NONE', #12841, #6033 ) ;
#1054 = DIRECTION ( 'NONE',  ( 0.000000000000000000, 0.000000000000000000, -1.000000000000000000 ) ) ;
#1055 = EDGE_LOOP ( 'NONE', ( #6384, #2925 ) ) ;
#1056 = PLANE ( 'NONE',  #12390 ) ;
#1057 = ORIENTED_EDGE ( 'NONE', *, *, #4752, .T. ) ;
#1058 = CARTESIAN_POINT ( 'NONE',  ( 1.000000000000000000, -5.473461295629626022, 0.000000000000000000 ) ) ;
#1059 = CARTESIAN_POINT ( 'NONE',  ( 50.72178482187501203, 62.76906990284730625, 4.503125000614517148 ) ) ;
#1060 = ORIENTED_EDGE ( 'NONE', *, *, #11229, .T. ) ;
#1061 = CARTESIAN_POINT ( 'NONE',  ( 66.44356964374998142, 108.1539533981018053, 4.671875000614517326 ) ) ;
#1062 = VECTOR ( 'NONE', #4789, 1000.000000000000000 ) ;
#1063 = EDGE_CURVE ( 'NONE', #11446, #10328, #11590, .T. ) ;
#1064 = CARTESIAN_POINT ( 'NONE',  ( 1.040000000000000036, -0.8660254037844385966, 0.4999999999999997780 ) ) ;
#1065 = CARTESIAN_POINT ( 'NONE',  ( 11.38811426945698635, 73.16316976839823383, 1.000000000000003109 ) ) ;
#1066 = SHAPE_REPRESENTATION ( 'lid', ( #5704 ), #60 ) ;
#1067 = ADVANCED_FACE ( 'NONE', ( #8724 ), #5714, .F. ) ;
#1068 = CARTESIAN_POINT ( 'NONE',  ( 17.54971918633085437, 66.83239978927272773, 4.000000000000000000 ) ) ;
#1069 = DIRECTION ( 'NONE',  ( 1.000000000000000000, 0.000000000000000000, 0.000000000000000000 ) ) ;
#1070=STYLED_ITEM('',(#12995),#11791);
#1071 = LINE ( 'NONE', #9053, #7641 ) ;
#1072 = DIRECTION ( 'NONE',  ( -1.000000000000000000, 0.000000000000000000, 0.000000000000000000 ) ) ;
#1073 = CARTESIAN_POINT ( 'NONE',  ( 3.556430356250015024, 90.00000000000000000, 3.509375000614517681 ) ) ;
#1074 = ORIENTED_EDGE ( 'NONE', *, *, #9115, .T. ) ;
#1075 = CARTESIAN_POINT ( 'NONE',  ( 3.800000000000004707, 90.00000000000000000, 6.000000000000000000 ) ) ;
#1076 = ORIENTED_EDGE ( 'NONE', *, *, #10227, .T. ) ;
#1077 = EDGE_CURVE ( 'NONE', #11420, #3844, #10237, .T. ) ;
#1078 = SURFACE_STYLE_FILL_AREA ( #217 ) ;
#1079 = CARTESIAN_POINT ( 'NONE',  ( -58.07179676972458537, 42.66025403784442460, -1.000000000000000000 ) ) ;
#1080 = CARTESIAN_POINT ( 'NONE',  ( 45.00000000000000000, -5.000000000000000000, -5.750000000000000000 ) ) ;
#1081 = CARTESIAN_POINT ( 'NONE',  ( 1.040000000000000036, -1.154700538379251240, 1.014316938424154191E-17 ) ) ;
#1082 = UNCERTAINTY_MEASURE_WITH_UNIT (LENGTH_MEASURE( 1.000000000000000082E-05 ), #4451, 'distance_accuracy_value', 'NONE');
#1083 = ORIENTED_EDGE ( 'NONE', *, *, #11509, .F. ) ;
#1084 = CARTESIAN_POINT ( 'NONE',  ( 1.000000000000000000, -4.873461295629625489, -0.8000000000000000444 ) ) ;
#1085 = DIRECTION ( 'NONE',  ( -0.000000000000000000, -1.000000000000000000, -0.000000000000000000 ) ) ;
#1086 = ORIENTED_EDGE ( 'NONE', *, *, #10661, .F. ) ;
#1087 = CIRCLE ( 'NONE', #457, 1.599999999999990319 ) ;
#1088 = CARTESIAN_POINT ( 'NONE',  ( -63.99999999999998579, 36.92820323027551410, -2.500000000000000000 ) ) ;
#1089 = ORIENTED_EDGE ( 'NONE', *, *, #8514, .F. ) ;
#1090 = SURFACE_STYLE_FILL_AREA ( #10057 ) ;
#1091 = ORIENTED_EDGE ( 'NONE', *, *, #8626, .F. ) ;
#1092 = ADVANCED_FACE ( 'NONE', ( #4448 ), #7017, .F. ) ;
#1093 = DIRECTION ( 'NONE',  ( 0.9510565162951530871, 0.3090169943749492276, 0.000000000000000000 ) ) ;
#1094 = PLANE ( 'NONE',  #2692 ) ;
#1095 = EDGE_LOOP ( 'NONE', ( #4761, #6603, #12509, #12056 ) ) ;
#1096 =( GEOMETRIC_REPRESENTATION_CONTEXT ( 3 ) GLOBAL_UNCERTAINTY_ASSIGNED_CONTEXT ( ( #6479 ) ) GLOBAL_UNIT_ASSIGNED_CONTEXT ( ( #3190, #9328, #152 ) ) REPRESENTATION_CONTEXT ( 'NONE', 'WORKASPACE' ) );
#1097 = ORIENTED_EDGE ( 'NONE', *, *, #1307, .F. ) ;
#1098 = CARTESIAN_POINT ( 'NONE',  ( 1.040000000000000036, 0.000000000000000000, 2.000000000000000000 ) ) ;
#1099 = ORIENTED_EDGE ( 'NONE', *, *, #12396, .F. ) ;
#1100 = EDGE_CURVE ( 'NONE', #8436, #7369, #1983, .T. ) ;
#1101 = APPLICATION_PROTOCOL_DEFINITION ( 'draft international standard', 'automotive_design', 1998, #7683 ) ;
#1102 = CARTESIAN_POINT ( 'NONE',  ( 19.27821517812500574, 117.2309300971526937, 2.928125000614517415 ) ) ;
#1103 = ADVANCED_FACE ( 'NONE', ( #9105 ), #8133, .T. ) ;
#1104 = VERTEX_POINT ( 'NONE', #5047 ) ;
#1105 = DIRECTION ( 'NONE',  ( 0.000000000000000000, 0.000000000000000000, 1.000000000000000000 ) ) ;
#1106 = VERTEX_POINT ( 'NONE', #10081 ) ;
#1107 =( GEOMETRIC_REPRESENTATION_CONTEXT ( 3 ) GLOBAL_UNCERTAINTY_ASSIGNED_CONTEXT ( ( #7087 ) ) GLOBAL_UNIT_ASSIGNED_CONTEXT ( ( #1952, #9928, #1155 ) ) REPRESENTATION_CONTEXT ( 'NONE', 'WORKASPACE' ) );
#1108 = DIRECTION ( 'NONE',  ( -0.000000000000000000, -0.000000000000000000, -1.000000000000000000 ) ) ;
#1109 = CARTESIAN_POINT ( 'NONE',  ( 66.44356964375000985, 71.84604660189820891, 4.090625000614517504 ) ) ;
#1110 = DIRECTION ( 'NONE',  ( 1.000000000000000000, 0.000000000000000000, 0.000000000000000000 ) ) ;
#1111 = CLOSED_SHELL ( 'NONE', ( #7998, #1318, #11759, #3374, #1067, #11979, #11060, #2711, #2077, #5346, #1103, #6314, #5407, #715, #7473, #6396, #5272, #6442, #10240, #7, #8396, #2560, #4373, #883, #6299, #12362, #3318 ) ) ;
#1112 = ADVANCED_FACE ( 'NONE', ( #1366, #12361, #1118 ), #3474, .T. ) ;
#1113 = CARTESIAN_POINT ( 'NONE',  ( 17.66025403784438197, 77.14656965084323303, 1.000000000000000000 ) ) ;
#1114 = ORIENTED_EDGE ( 'NONE', *, *, #12529, .F. ) ;
#1115 = PRODUCT_DEFINITION_FORMATION_WITH_SPECIFIED_SOURCE ( 'ANY', '', #8459, .NOT_KNOWN. ) ;
#1116 = CARTESIAN_POINT ( 'NONE',  ( 3.800000000000025135, 71.98667160128366049, 3.237500000000000266 ) ) ;
#1117 = DIRECTION ( 'NONE',  ( 0.000000000000000000, 1.000000000000000000, 0.000000000000000000 ) ) ;
#1118 = FACE_BOUND ( 'NONE', #9389, .T. ) ;
#1119 = EDGE_LOOP ( 'NONE', ( #1583, #11044, #4776, #9799 ) ) ;
#1120 = EDGE_CURVE ( 'NONE', #11429, #7517, #11126, .T. ) ;
#1121 = VECTOR ( 'NONE', #8149, 1000.000000000000000 ) ;
#1122 = ORIENTED_EDGE ( 'NONE', *, *, #81, .F. ) ;
#1123 = VECTOR ( 'NONE', #2979, 1000.000000000000000 ) ;
#1124 = DIRECTION ( 'NONE',  ( 0.000000000000000000, 1.000000000000000000, -1.370729058197317775E-18 ) ) ;
#1125 = CARTESIAN_POINT ( 'NONE',  ( 3.556430356250015024, 90.00000000000000000, 4.353125000614517681 ) ) ;
#1126 = ORIENTED_EDGE ( 'NONE', *, *, #8124, .T. ) ;
#1127 = CARTESIAN_POINT ( 'NONE',  ( 66.44356964374999563, 71.84604660189820891, 3.696875000614517237 ) ) ;
#1128 = FACE_OUTER_BOUND ( 'NONE', #1276, .T. ) ;
#1129 = CARTESIAN_POINT ( 'NONE',  ( -2.387319993259524598, -4.036502139894371233, -0.8000000000000000444 ) ) ;
#1130 = VECTOR ( 'NONE', #208, 1000.000000000000000 ) ;
#1131 = CIRCLE ( 'NONE', #10551, 1.500000000000001332 ) ;
#1132 = DIRECTION ( 'NONE',  ( -1.000000000000000000, 0.000000000000000000, 0.000000000000000000 ) ) ;
#1133 = CARTESIAN_POINT ( 'NONE',  ( 1.649999999999999023, 0.000000000000000000, 0.000000000000000000 ) ) ;
#1134 = DIRECTION ( 'NONE',  ( 0.000000000000000000, 0.000000000000000000, 1.000000000000000000 ) ) ;
#1135 = FACE_OUTER_BOUND ( 'NONE', #11908, .T. ) ;
#1136 = LINE ( 'NONE', #145, #7950 ) ;
#1137 = VECTOR ( 'NONE', #8632, 1000.000000000000000 ) ;
#1138 = LINE ( 'NONE', #9124, #5567 ) ;
#1139 = EDGE_CURVE ( 'NONE', #7089, #12205, #10997, .T. ) ;
#1140 = VERTEX_POINT ( 'NONE', #7386 ) ;
#1141 = AXIS2_PLACEMENT_3D ( 'NONE', #1428, #3600, #12425 ) ;
#1142 = DIRECTION ( 'NONE',  ( -0.000000000000000000, 0.000000000000000000, 1.000000000000000000 ) ) ;
#1143 = EDGE_LOOP ( 'NONE', ( #5966, #12184, #3162, #12895 ) ) ;
#1144 = DIRECTION ( 'NONE',  ( -0.8660254037844360431, -0.5000000000000047740, -0.000000000000000000 ) ) ;
#1145 = CARTESIAN_POINT ( 'NONE',  ( 25.00000000000000355, -5.901290925839664858, 5.750000000000000000 ) ) ;
#1146 = CIRCLE ( 'NONE', #2418, 1.599999999999990319 ) ;
#1147 = PRODUCT_DEFINITION_SHAPE ( 'NONE', 'NONE',  #12965 ) ;
#1148 = CARTESIAN_POINT ( 'NONE',  ( 33.90709641728108892, 93.16671150547063007, 4.000000000000000000 ) ) ;
#1149 = AXIS2_PLACEMENT_3D ( 'NONE', #11024, #8159, #2079 ) ;
#1150 = ORIENTED_EDGE ( 'NONE', *, *, #3390, .T. ) ;
#1151 = CARTESIAN_POINT ( 'NONE',  ( 3.350000000000000089, 0.000000000000000000, -0.8000000000000000444 ) ) ;
#1152 = CARTESIAN_POINT ( 'NONE',  ( 66.20000000000008811, 108.0133283987162542, 4.025000001229034119 ) ) ;
#1153 = EDGE_CURVE ( 'NONE', #2281, #8808, #11372, .T. ) ;
#1154 = VERTEX_POINT ( 'NONE', #11439 ) ;
#1155 =( NAMED_UNIT ( * ) SI_UNIT ( $, .STERADIAN. ) SOLID_ANGLE_UNIT ( ) );
#1156 = DIRECTION ( 'NONE',  ( 0.000000000000000000, 0.000000000000000000, 1.000000000000000000 ) ) ;
#1157 = EDGE_CURVE ( 'NONE', #11476, #11262, #3029, .T. ) ;
#1158 = EDGE_LOOP ( 'NONE', ( #7100, #8756, #5861, #11911, #2951, #5490, #7151, #3080, #5486, #5090, #126, #8702 ) ) ;
#1159 = SURFACE_SIDE_STYLE ('',( #1090 ) ) ;
#1161 = ORIENTED_EDGE ( 'NONE', *, *, #4184, .T. ) ;
#1160 = VECTOR ( 'NONE', #10888, 1000.000000000000000 ) ;
#1162 = AXIS2_PLACEMENT_3D ( 'NONE', #1080, #9331, #5271 ) ;
#1163 = CARTESIAN_POINT ( 'NONE',  ( 3.800000000000015810, 108.0133283987162969, 4.625000001229034652 ) ) ;
#1164 = DIRECTION ( 'NONE',  ( 0.000000000000000000, 0.000000000000000000, -1.000000000000000000 ) ) ;
#1165 = ORIENTED_EDGE ( 'NONE', *, *, #10513, .T. ) ;
#1166 = EDGE_LOOP ( 'NONE', ( #412, #7388 ) ) ;
#1167 = DIRECTION ( 'NONE',  ( -1.000000000000000000, 0.000000000000000000, 0.000000000000000000 ) ) ;
#1168 = ORIENTED_EDGE ( 'NONE', *, *, #4161, .T. ) ;
#1169 = PRODUCT_CONTEXT ( 'NONE', #10180, 'mechanical' ) ;
#1170 = CARTESIAN_POINT ( 'NONE',  ( 66.19999999999998863, 90.00000000000000000, 4.437500001229033764 ) ) ;
#1171 = EDGE_CURVE ( 'NONE', #11574, #9287, #1498, .T. ) ;
#1172 = CIRCLE ( 'NONE', #3276, 3.499999999999996003 ) ;
#1173 = ORIENTED_EDGE ( 'NONE', *, *, #6921, .F. ) ;
#1174 = DIRECTION ( 'NONE',  ( 1.000000000000000000, 0.000000000000000000, -0.000000000000000000 ) ) ;
#1175 = CYLINDRICAL_SURFACE ( 'NONE', #1863, 1.499999999999999556 ) ;
#1176 = ORIENTED_EDGE ( 'NONE', *, *, #9094, .T. ) ;
#1177 = LINE ( 'NONE', #6217, #1912 ) ;
#1178 = CARTESIAN_POINT ( 'NONE',  ( 50.72178482187501203, 62.76906990284730625, 4.053125000614517859 ) ) ;
#1179 = CARTESIAN_POINT ( 'NONE',  ( 35.00000000000000000, 126.0266567974326222, 3.200000001229034385 ) ) ;
#1180 = LINE ( 'NONE', #250, #9978 ) ;
#1181 = PRESENTATION_STYLE_ASSIGNMENT (( #10144 ) ) ;
#1182 = VECTOR ( 'NONE', #5508, 1000.000000000000114 ) ;
#1183 = CARTESIAN_POINT ( 'NONE',  ( 35.00000000000000000, 90.00000000000000000, 6.000000000000000000 ) ) ;
#1184 = VERTEX_POINT ( 'NONE', #10716 ) ;
#1185 = CARTESIAN_POINT ( 'NONE',  ( 50.59999999999999432, 117.0199925980744666, 3.500000000000000444 ) ) ;
#1186 = ORIENTED_EDGE ( 'NONE', *, *, #10214, .F. ) ;
#1187 = DIRECTION ( 'NONE',  ( -0.000000000000000000, -1.000000000000000000, -0.000000000000000000 ) ) ;
#1188 = EDGE_LOOP ( 'NONE', ( #638, #12953, #4691 ) ) ;
#1189 = CARTESIAN_POINT ( 'NONE',  ( 20.00000000000000355, 121.2009999999999934, 1.500000000000000444 ) ) ;
#1190 = ORIENTED_EDGE ( 'NONE', *, *, #12704, .T. ) ;
#1191 = VECTOR ( 'NONE', #4790, 1000.000000000000227 ) ;
#1192 = CARTESIAN_POINT ( 'NONE',  ( 1.617350269189632428, 0.000000000000000000, 0.000000000000000000 ) ) ;
#1193 = UNCERTAINTY_MEASURE_WITH_UNIT (LENGTH_MEASURE( 1.000000000000000082E-05 ), #9138, 'distance_accuracy_value', 'NONE');
#1194 = CARTESIAN_POINT ( 'NONE',  ( 66.44356964374998142, 108.1539533981018053, 4.165625000614516793 ) ) ;
#1195 = ORIENTED_EDGE ( 'NONE', *, *, #453, .T. ) ;
#1196 = CARTESIAN_POINT ( 'NONE',  ( 3.556430356250015024, 90.00000000000000000, 4.859375000614517326 ) ) ;
#1197 = CARTESIAN_POINT ( 'NONE',  ( 62.42613047537196991, 99.43702109502110886, -1.000000000000000000 ) ) ;
#1198 = EDGE_CURVE ( 'NONE', #9926, #4325, #8868, .T. ) ;
#1199 = DIRECTION ( 'NONE',  ( -0.000000000000000000, -0.000000000000000000, -1.000000000000000000 ) ) ;
#1200 = EDGE_CURVE ( 'NONE', #11292, #11250, #10783, .T. ) ;
#1201 = AXIS2_PLACEMENT_3D ( 'NONE', #8859, #2915, #336 ) ;
#1202 = CARTESIAN_POINT ( 'NONE',  ( 35.75000000000000711, 93.41869858279433458, 4.000000000000000000 ) ) ;
#1203 = CARTESIAN_POINT ( 'NONE',  ( 35.00000000000000000, 90.00000000000000000, 4.000000000000000000 ) ) ;
#1204 = CARTESIAN_POINT ( 'NONE',  ( 34.49999999999995026, 119.0000000000000000, -1.000000000000000000 ) ) ;
#1205 = DIRECTION ( 'NONE',  ( -0.000000000000000000, 0.000000000000000000, 1.000000000000000000 ) ) ;
#1206 = DIRECTION ( 'NONE',  ( -0.000000000000000000, -0.000000000000000000, -1.000000000000000000 ) ) ;
#1207 = DIRECTION ( 'NONE',  ( 0.000000000000000000, 0.4999999999999998890, 0.8660254037844387076 ) ) ;
#1208 = VECTOR ( 'NONE', #3192, 1000.000000000000000 ) ;
#1209 = VERTEX_POINT ( 'NONE', #4643 ) ;
#1210 = VECTOR ( 'NONE', #2174, 1000.000000000000000 ) ;
#1211 = CARTESIAN_POINT ( 'NONE',  ( 34.25000000000000000, 93.41869858279433458, 4.800000000000000711 ) ) ;
#1212 = ORIENTED_EDGE ( 'NONE', *, *, #4918, .T. ) ;
#1213 = FILL_AREA_STYLE_COLOUR ( '', #7165 ) ;
#1214 = DIRECTION ( 'NONE',  ( -1.000000000000000000, -0.000000000000000000, -0.000000000000000000 ) ) ;
#1215 = FACE_OUTER_BOUND ( 'NONE', #9863, .T. ) ;
#1216 = EDGE_CURVE ( 'NONE', #1668, #4783, #721, .T. ) ;
#1217 = CARTESIAN_POINT ( 'NONE',  ( 7.500000000000000000, 34.99999999999999289, 0.000000000000000000 ) ) ;
#1218 = AXIS2_PLACEMENT_3D ( 'NONE', #11961, #967, #235 ) ;
#1219 = ORIENTED_EDGE ( 'NONE', *, *, #11969, .T. ) ;
#1220 = CARTESIAN_POINT ( 'NONE',  ( 35.00000000000000000, 90.00000000000000000, 4.000000000000000000 ) ) ;
#1221 = CARTESIAN_POINT ( 'NONE',  ( -60.38397459621555186, 30.66506350946108128, 0.000000000000000000 ) ) ;
#1222 = ORIENTED_EDGE ( 'NONE', *, *, #48, .F. ) ;
#1223 = DIRECTION ( 'NONE',  ( 5.624500927088228034E-17, -1.370729058197317775E-18, -1.000000000000000000 ) ) ;
#1224 = VERTEX_POINT ( 'NONE', #5684 ) ;
#1225 = CARTESIAN_POINT ( 'NONE',  ( 34.25000000000000000, 93.50000000000000000, -4.802775637732004554 ) ) ;
#1226 = ORIENTED_EDGE ( 'NONE', *, *, #12302, .T. ) ;
#1227 = AXIS2_PLACEMENT_3D ( 'NONE', #3244, #11210, #139 ) ;
#1228 = PLANE ( 'NONE',  #11328 ) ;
#1229 = DIRECTION ( 'NONE',  ( 0.8660254037844361541, 0.5000000000000042188, 0.000000000000000000 ) ) ;
#1230 = EDGE_CURVE ( 'NONE', #5275, #1050, #1631, .T. ) ;
#1231 = ORIENTED_EDGE ( 'NONE', *, *, #5801, .T. ) ;
#1232 = PRODUCT_DEFINITION_CONTEXT ( 'detailed design', #12541, 'design' ) ;
#1233 = EDGE_CURVE ( 'NONE', #11967, #3765, #2195, .T. ) ;
#1234 = ORIENTED_EDGE ( 'NONE', *, *, #11061, .F. ) ;
#1236 = DIRECTION ( 'NONE',  ( 0.000000000000000000, 0.000000000000000000, 1.000000000000000000 ) ) ;
#1235 = CIRCLE ( 'NONE', #10439, 3.349999999999995204 ) ;
#1237 = ORIENTED_EDGE ( 'NONE', *, *, #9652, .F. ) ;
#1238 = CARTESIAN_POINT ( 'NONE',  ( 35.00000000000000000, 126.3079067962035822, 3.790625000614517237 ) ) ;
#1239 = AXIS2_PLACEMENT_3D ( 'NONE', #7208, #5306, #5243 ) ;
#1240 = ORIENTED_EDGE ( 'NONE', *, *, #11905, .F. ) ;
#1241 = APPLICATION_CONTEXT ( 'automotive_design' ) ;
#1242 = CARTESIAN_POINT ( 'NONE',  ( 66.19999999999998863, 90.00000000000000000, 3.537500001229034297 ) ) ;
#1243 = DIRECTION ( 'NONE',  ( -0.000000000000000000, -1.000000000000000000, -0.000000000000000000 ) ) ;
#1244 = ORIENTED_EDGE ( 'NONE', *, *, #5393, .F. ) ;
#1245 = LINE ( 'NONE', #182, #645 ) ;
#1246 = CARTESIAN_POINT ( 'NONE',  ( 3.556430356250014579, 108.1539533981018053, 3.415625000614516793 ) ) ;
#1247 = FACE_BOUND ( 'NONE', #3736, .T. ) ;
#1248 = AXIS2_PLACEMENT_3D ( 'NONE', #1741, #5729, #4754 ) ;
#1249 = CARTESIAN_POINT ( 'NONE',  ( 66.19999999999998863, 90.00000000000000000, 3.087500001229034119 ) ) ;
#1250 = EDGE_CURVE ( 'NONE', #8496, #7310, #9672, .T. ) ;
#1251 = CARTESIAN_POINT ( 'NONE',  ( -48.33333333333332860, 2.000000000000001332, -1.599999999999992095 ) ) ;
#1252 = ORIENTED_EDGE ( 'NONE', *, *, #1576, .T. ) ;
#1253 = CARTESIAN_POINT ( 'NONE',  ( 50.59999999999999432, 117.0199925980744666, 4.400000000000000355 ) ) ;
#1254 = EDGE_LOOP ( 'NONE', ( #7238, #10734, #387, #7725 ) ) ;
#1255 = CARTESIAN_POINT ( 'NONE',  ( 34.25000000000000000, 92.49999999999998579, -3.000000000000000000 ) ) ;
#1256 = ORIENTED_EDGE ( 'NONE', *, *, #8645, .T. ) ;
#1257 = AXIS2_PLACEMENT_3D ( 'NONE', #12940, #5020, #6193 ) ;
#1258 = CARTESIAN_POINT ( 'NONE',  ( 1.000000000000000000, -4.873461295629625489, -0.8000000000000000444 ) ) ;
#1259 = ORIENTED_EDGE ( 'NONE', *, *, #11539, .T. ) ;
#1260 = CARTESIAN_POINT ( 'NONE',  ( -3.068288344391240763, -2.655262421758692426, 0.000000000000000000 ) ) ;
#1261 = CARTESIAN_POINT ( 'NONE',  ( 3.556430356250014579, 108.1539533981018053, 4.315625000614517148 ) ) ;
#1262 = CARTESIAN_POINT ( 'NONE',  ( 66.44356964375000985, 71.84604660189820891, 4.596875000614516260 ) ) ;
#1263 = CARTESIAN_POINT ( 'NONE',  ( 3.033375984251970081, -8.673617379884035472E-16, 0.000000000000000000 ) ) ;
#1264 = EDGE_CURVE ( 'NONE', #10380, #9690, #768, .T. ) ;
#1265 = CARTESIAN_POINT ( 'NONE',  ( 1.000000000000000000, -5.473461295629626022, 0.000000000000000000 ) ) ;
#1266 = CIRCLE ( 'NONE', #5015, 0.7499999999999997780 ) ;
#1267 = DIRECTION ( 'NONE',  ( 1.000000000000000000, 0.000000000000000000, -0.000000000000000000 ) ) ;
#1268 = CYLINDRICAL_SURFACE ( 'NONE', #7741, 28.99999999999999289 ) ;
#1269 = CARTESIAN_POINT ( 'NONE',  ( 50.00000000000000000, 0.000000000000000000, 10.00000000000000000 ) ) ;
#1270 = CARTESIAN_POINT ( 'NONE',  ( 7.500000000000000000, 34.99999999999999289, 0.000000000000000000 ) ) ;
#1271 = EDGE_CURVE ( 'NONE', #8824, #5732, #8757, .T. ) ;
#1272 = EDGE_CURVE ( 'NONE', #9602, #3240, #4770, .T. ) ;
#1273 = VECTOR ( 'NONE', #9896, 1000.000000000000000 ) ;
#1274 = DIRECTION ( 'NONE',  ( -0.9549484348006339607, -0.2967717757331703732, 0.000000000000000000 ) ) ;
#1275 = CARTESIAN_POINT ( 'NONE',  ( 0.000000000000000000, 0.000000000000000000, 0.000000000000000000 ) ) ;
#1276 = EDGE_LOOP ( 'NONE', ( #4208, #71, #3279, #2759 ) ) ;
#1277 = DIRECTION ( 'NONE',  ( -0.000000000000000000, -0.000000000000000000, -1.000000000000000000 ) ) ;
#1278 = VERTEX_POINT ( 'NONE', #4514 ) ;
#1279 = EDGE_CURVE ( 'NONE', #7668, #8436, #12840, .T. ) ;
#1280 = AXIS2_PLACEMENT_3D ( 'NONE', #7330, #12243, #1438 ) ;
#1281 = CARTESIAN_POINT ( 'NONE',  ( 51.64126381929429499, 66.24461453698036451, -1.000000000000000000 ) ) ;
#1282 = DIRECTION ( 'NONE',  ( 0.8660254037844365982, 0.5000000000000036637, -0.000000000000000000 ) ) ;
#1283 = CARTESIAN_POINT ( 'NONE',  ( 1.040000000000000036, 0.8660254037844390407, 0.5000000000000002220 ) ) ;
#1284 = ORIENTED_EDGE ( 'NONE', *, *, #4752, .F. ) ;
#1285 = LINE ( 'NONE', #7245, #3044 ) ;
#1286 = CARTESIAN_POINT ( 'NONE',  ( -61.88397459621555186, 33.26313972081440085, 1.836970198721030427E-16 ) ) ;
#1287 = EDGE_LOOP ( 'NONE', ( #8218, #2510 ) ) ;
#1288 = SURFACE_STYLE_FILL_AREA ( #1483 ) ;
#1289 = LINE ( 'NONE', #6262, #7232 ) ;
#1290 = ORIENTED_EDGE ( 'NONE', *, *, #5724, .F. ) ;
#1291 = COLOUR_RGB ( '',0.8941176470588234615, 0.8941176470588234615, 0.8941176470588234615 ) ;
#1292 = VERTEX_POINT ( 'NONE', #10596 ) ;
#1293 = EDGE_CURVE ( 'NONE', #4584, #1989, #12495, .T. ) ;
#1294 = CARTESIAN_POINT ( 'NONE',  ( -60.00000000000000000, 30.00000000000000000, 7.999999999999996447 ) ) ;
#1295 = DIRECTION ( 'NONE',  ( -0.000000000000000000, 0.5000000000000003331, 0.8660254037844384856 ) ) ;
#1296 = ORIENTED_EDGE ( 'NONE', *, *, #3497, .F. ) ;
#1297 = EDGE_LOOP ( 'NONE', ( #7827, #837, #9546, #8819, #11893, #3996 ) ) ;
#1298 = VECTOR ( 'NONE', #9824, 1000.000000000000000 ) ;
#1299 = CARTESIAN_POINT ( 'NONE',  ( 52.49999999999996447, 90.00000000000000000, -10.00000000000000000 ) ) ;
#1300 = EDGE_LOOP ( 'NONE', ( #9011, #8775, #11719, #6124 ) ) ;
#1301 = DIRECTION ( 'NONE',  ( 1.127570259384924611E-17, -1.000000000000000000, 0.000000000000000000 ) ) ;
#1302 = CARTESIAN_POINT ( 'NONE',  ( 3.556430356250015024, 90.00000000000000000, 3.453125000614517770 ) ) ;
#1303 = ORIENTED_EDGE ( 'NONE', *, *, #1642, .T. ) ;
#1304 = DIRECTION ( 'NONE',  ( 0.03100775193798453039, 0.9995191440486532741, -0.000000000000000000 ) ) ;
#1305 = ORIENTED_EDGE ( 'NONE', *, *, #12229, .T. ) ;
#1306 = FACE_OUTER_BOUND ( 'NONE', #7469, .T. ) ;
#1307 = EDGE_CURVE ( 'NONE', #2471, #5455, #12751, .T. ) ;
#1308 = CARTESIAN_POINT ( 'NONE',  ( 3.800000000000015365, 90.00000000000000000, 4.549999999999999822 ) ) ;
#1309 = CARTESIAN_POINT ( 'NONE',  ( 9.999999999999994671, 30.00000000000000000, -2.500000000000000000 ) ) ;
#1310 =( NAMED_UNIT ( * ) PLANE_ANGLE_UNIT ( ) SI_UNIT ( $, .RADIAN. ) );
#1311 = DIRECTION ( 'NONE',  ( 5.624500927088228034E-17, -1.370729058197317775E-18, -1.000000000000000000 ) ) ;
#1312 = ORIENTED_EDGE ( 'NONE', *, *, #1891, .T. ) ;
#1313 = CARTESIAN_POINT ( 'NONE',  ( 3.556430356250014579, 108.1539533981018053, 4.371875000614517504 ) ) ;
#1314 = LINE ( 'NONE', #10350, #3761 ) ;
#1315 = ORIENTED_EDGE ( 'NONE', *, *, #9075, .F. ) ;
#1316 = DIRECTION ( 'NONE',  ( 0.000000000000000000, 0.000000000000000000, -1.000000000000000000 ) ) ;
#1317 = ORIENTED_EDGE ( 'NONE', *, *, #10037, .F. ) ;
#1318 = ADVANCED_FACE ( 'NONE', ( #7771 ), #1564, .T. ) ;
#1319 = CARTESIAN_POINT ( 'NONE',  ( -67.46410161513773573, 36.92820323027551410, 2.500000000000000000 ) ) ;
#1320 = AXIS2_PLACEMENT_3D ( 'NONE', #7964, #5805, #9918 ) ;
#1321 = CARTESIAN_POINT ( 'NONE',  ( 6.262912888864590855, 102.7722879626690400, 3.000000000000000888 ) ) ;
#1322 = ADVANCED_FACE ( 'NONE', ( #5552 ), #9549, .T. ) ;
#1323 = DIRECTION ( 'NONE',  ( 0.000000000000000000, -1.000000000000000000, 0.000000000000000000 ) ) ;
#1324 = CARTESIAN_POINT ( 'NONE',  ( 35.00000000000000000, 90.00000000000000000, 4.000000000000000000 ) ) ;
#1325 = DIRECTION ( 'NONE',  ( -1.000000000000000000, 0.000000000000000000, 0.000000000000000000 ) ) ;
#1326 = PRESENTATION_LAYER_ASSIGNMENT (  '', '', ( #10095 ) ) ;
#1327 = AXIS2_PLACEMENT_3D ( 'NONE', #5273, #7305, #8292 ) ;
#1328 = LINE ( 'NONE', #12388, #3779 ) ;
#1329 = FACE_OUTER_BOUND ( 'NONE', #9005, .T. ) ;
#1330 = DIRECTION ( 'NONE',  ( 1.000000000000000000, 0.000000000000000000, 5.337610695313252124E-17 ) ) ;
#1331 = EDGE_CURVE ( 'NONE', #307, #4218, #12687, .T. ) ;
#1332 = AXIS2_PLACEMENT_3D ( 'NONE', #9271, #4566, #360 ) ;
#1333 = LINE ( 'NONE', #9323, #4401 ) ;
#1334 = CARTESIAN_POINT ( 'NONE',  ( 20.00000000000000355, 2.000000000000000000, 10.00000000000000000 ) ) ;
#1335 = ORIENTED_EDGE ( 'NONE', *, *, #5063, .F. ) ;
#1336 = DIRECTION ( 'NONE',  ( 0.000000000000000000, 0.000000000000000000, -1.000000000000000000 ) ) ;
#1337 = ORIENTED_EDGE ( 'NONE', *, *, #10803, .F. ) ;
#1338 = VECTOR ( 'NONE', #6044, 1000.000000000000000 ) ;
#1339 = PRODUCT ( 'wheel support and navigator', 'wheel support and navigator', '', ( #4192 ) ) ;
#1340 = DIRECTION ( 'NONE',  ( 0.000000000000000000, 1.000000000000000000, 0.000000000000000000 ) ) ;
#1341 = AXIS2_PLACEMENT_3D ( 'NONE', #7691, #5529, #617 ) ;
#1342 = ADVANCED_FACE ( 'NONE', ( #8575 ), #1756, .T. ) ;
#1343 = LINE ( 'NONE', #9197, #12715 ) ;
#1344 = PLANE ( 'NONE',  #941 ) ;
#1345 = FACE_OUTER_BOUND ( 'NONE', #11526, .T. ) ;
#1346 = ORIENTED_EDGE ( 'NONE', *, *, #2870, .F. ) ;
#1347 = AXIS2_PLACEMENT_3D ( 'NONE', #6885, #3700, #797 ) ;
#1348 = FACE_OUTER_BOUND ( 'NONE', #2904, .T. ) ;
#1349 = DIRECTION ( 'NONE',  ( 0.000000000000000000, 0.000000000000000000, -1.000000000000000000 ) ) ;
#1350 = AXIS2_PLACEMENT_3D ( 'NONE', #2842, #6816, #8722 ) ;
#1351 = VERTEX_POINT ( 'NONE', #3602 ) ;
#1352 = CARTESIAN_POINT ( 'NONE',  ( -58.07179676972457116, 42.66025403784438907, 1.000000000000000000 ) ) ;
#1353 = VERTEX_POINT ( 'NONE', #7583 ) ;
#1354 = ORIENTED_EDGE ( 'NONE', *, *, #8514, .T. ) ;
#1355 = DIRECTION ( 'NONE',  ( 0.000000000000000000, 0.000000000000000000, -1.000000000000000000 ) ) ;
#1356 = DIRECTION ( 'NONE',  ( -0.000000000000000000, 1.000000000000000000, -0.000000000000000000 ) ) ;
#1357 = CIRCLE ( 'NONE', #12227, 3.500000000000003109 ) ;
#1358 = ORIENTED_EDGE ( 'NONE', *, *, #6254, .F. ) ;
#1359 = PRODUCT_DEFINITION_CONTEXT ( 'detailed design', #232, 'design' ) ;
#1360 = EDGE_CURVE ( 'NONE', #5732, #10262, #11699, .T. ) ;
#1361 = EDGE_CURVE ( 'NONE', #7045, #2314, #5869, .T. ) ;
#1362 = AXIS2_PLACEMENT_3D ( 'NONE', #3082, #7982, #8050 ) ;
#1363 = ORIENTED_EDGE ( 'NONE', *, *, #917, .F. ) ;
#1364 = LINE ( 'NONE', #435, #5330 ) ;
#1365 = ORIENTED_EDGE ( 'NONE', *, *, #8234, .T. ) ;
#1366 = FACE_OUTER_BOUND ( 'NONE', #429, .T. ) ;
#1367 =( LENGTH_UNIT ( ) NAMED_UNIT ( * ) SI_UNIT ( .MILLI., .METRE. ) );
#1368 = CARTESIAN_POINT ( 'NONE',  ( 66.19999999999998863, 90.00000000000000000, 3.425000000000000266 ) ) ;
#1369 = ORIENTED_EDGE ( 'NONE', *, *, #5464, .F. ) ;
#1370 = AXIS2_PLACEMENT_3D ( 'NONE', #3051, #11936, #5062 ) ;
#1371 = DIRECTION ( 'NONE',  ( 0.000000000000000000, -0.000000000000000000, 1.000000000000000000 ) ) ;
#1372 = ORIENTED_EDGE ( 'NONE', *, *, #6536, .T. ) ;
#1373 = AXIS2_PLACEMENT_3D ( 'NONE', #12342, #12472, #9393 ) ;
#1374 = ADVANCED_BREP_SHAPE_REPRESENTATION ( '', ( #3541, #5704 ), #11138 ) ;
#1375 = CARTESIAN_POINT ( 'NONE',  ( 1.040000000000000036, 0.8660254037844393737, 0.5000000000000007772 ) ) ;
#1376 = DIRECTION ( 'NONE',  ( 0.000000000000000000, -1.000000000000000000, -0.000000000000000000 ) ) ;
#1377 = DIRECTION ( 'NONE',  ( 0.000000000000000000, 0.000000000000000000, 1.000000000000000000 ) ) ;
#1378 = ORIENTED_EDGE ( 'NONE', *, *, #3459, .T. ) ;
#1379 = AXIS2_PLACEMENT_3D ( 'NONE', #8945, #961, #3988 ) ;
#1380 = CARTESIAN_POINT ( 'NONE',  ( 50.72178482187501203, 62.76906990284730625, 3.659375000614517592 ) ) ;
#1381 = ORIENTED_EDGE ( 'NONE', *, *, #6577, .T. ) ;
#1382 = EDGE_CURVE ( 'NONE', #5549, #3421, #6570, .T. ) ;
#1383 = CARTESIAN_POINT ( 'NONE',  ( -9.666666666666658969, 61.36936462597000741, 0.9999999999999997780 ) ) ;
#1384 = ORIENTED_EDGE ( 'NONE', *, *, #3350, .F. ) ;
#1385 = FACE_OUTER_BOUND ( 'NONE', #5050, .T. ) ;
#1386 = ORIENTED_EDGE ( 'NONE', *, *, #1264, .F. ) ;
#1387 = DIRECTION ( 'NONE',  ( -0.000000000000000000, 1.000000000000000000, -0.000000000000000000 ) ) ;
#1388 = CARTESIAN_POINT ( 'NONE',  ( 35.00000000000000000, 90.00000000000000000, -1.000000000000000888 ) ) ;
#1389 = AXIS2_PLACEMENT_3D ( 'NONE', #11217, #11017, #146 ) ;
#1390 = CARTESIAN_POINT ( 'NONE',  ( 50.72178482187501203, 62.76906990284730625, 3.209375000614517415 ) ) ;
#1391 = DIRECTION ( 'NONE',  ( -0.000000000000000000, 0.4999999999999998890, -0.8660254037844387076 ) ) ;
#1392 = DIRECTION ( 'NONE',  ( -0.000000000000000000, -0.000000000000000000, -1.000000000000000000 ) ) ;
#1393 = EDGE_CURVE ( 'NONE', #11615, #4578, #5928, .T. ) ;
#1394 = DIRECTION ( 'NONE',  ( -0.000000000000000000, -0.000000000000000000, -1.000000000000000000 ) ) ;
#1395 = ADVANCED_FACE ( 'NONE', ( #7838 ), #9861, .F. ) ;
#1396 = DIRECTION ( 'NONE',  ( 0.000000000000000000, -0.5000000000000003331, 0.8660254037844383745 ) ) ;
#1397 = ADVANCED_FACE ( 'NONE', ( #2997 ), #11830, .F. ) ;
#1398 = DIRECTION ( 'NONE',  ( 1.000000000000000000, 0.000000000000000000, 0.000000000000000000 ) ) ;
#1399 = CARTESIAN_POINT ( 'NONE',  ( 1.749999999999999112, 0.000000000000000000, 0.000000000000000000 ) ) ;
#1400 = CIRCLE ( 'NONE', #8716, 6.499999999999999112 ) ;
#1401 = DIRECTION ( 'NONE',  ( -0.8660254037844361541, -0.5000000000000042188, 0.000000000000000000 ) ) ;
#1402 = CARTESIAN_POINT ( 'NONE',  ( 35.00000000000000000, 90.00000000000000000, -1.000000000000000000 ) ) ;
#1403 = CARTESIAN_POINT ( 'NONE',  ( 3.800000000000015365, 90.00000000000000000, 3.762500001229034385 ) ) ;
#1404 = ORIENTED_EDGE ( 'NONE', *, *, #12529, .T. ) ;
#1405 = DIRECTION ( 'NONE',  ( -1.000000000000000000, 0.000000000000000000, 0.000000000000000000 ) ) ;
#1406 = ORIENTED_EDGE ( 'NONE', *, *, #6522, .T. ) ;
#1407 = VECTOR ( 'NONE', #3256, 1000.000000000000000 ) ;
#1408 =( LENGTH_UNIT ( ) NAMED_UNIT ( * ) SI_UNIT ( .MILLI., .METRE. ) );
#1409 = EDGE_CURVE ( 'NONE', #3535, #10249, #5810, .T. ) ;
#1410 = FACE_OUTER_BOUND ( 'NONE', #10954, .T. ) ;
#1411 = CARTESIAN_POINT ( 'NONE',  ( 20.00000000000000355, 2.000000000000000000, 10.00000000000000000 ) ) ;
#1412 = CARTESIAN_POINT ( 'NONE',  ( 3.800000000000015365, 90.00000000000000000, 3.650000000000000355 ) ) ;
#1413 = VERTEX_POINT ( 'NONE', #1886 ) ;
#1414 = DIRECTION ( 'NONE',  ( -1.000000000000000000, 0.000000000000000000, 0.000000000000000000 ) ) ;
#1415 = CARTESIAN_POINT ( 'NONE',  ( 50.72178482187499071, 117.2309300971526937, 4.653125000614517504 ) ) ;
#1416 = AXIS2_PLACEMENT_3D ( 'NONE', #12045, #10076, #4203 ) ;
#1417 = EDGE_LOOP ( 'NONE', ( #9875, #11327, #1315, #8579, #2320, #12149 ) ) ;
#1418 = CARTESIAN_POINT ( 'NONE',  ( 35.00000000000000000, 90.00000000000000000, -3.000000000000000000 ) ) ;
#1419 = EDGE_LOOP ( 'NONE', ( #8931, #6655, #498, #10152 ) ) ;
#1420 = ORIENTED_EDGE ( 'NONE', *, *, #6430, .F. ) ;
#1421 = CARTESIAN_POINT ( 'NONE',  ( 30.00000000000000711, 0.000000000000000000, -1.499999999999999778 ) ) ;
#1422 = LINE ( 'NONE', #7513, #9367 ) ;
#1423 = CONICAL_SURFACE ( 'NONE', #8325, 1.500000000000003331, 1.029744259999999967 ) ;
#1424 = ORIENTED_EDGE ( 'NONE', *, *, #2897, .T. ) ;
#1425 = EDGE_CURVE ( 'NONE', #10706, #1636, #1146, .T. ) ;
#1426 = VECTOR ( 'NONE', #3530, 999.9999999999998863 ) ;
#1427 = VERTEX_POINT ( 'NONE', #4956 ) ;
#1428 = CARTESIAN_POINT ( 'NONE',  ( 35.00000000000000000, 90.00000000000000000, 4.800000000000000711 ) ) ;
#1429 = ORIENTED_EDGE ( 'NONE', *, *, #5239, .T. ) ;
#1430 = CARTESIAN_POINT ( 'NONE',  ( 57.53855666881469233, 111.6893844235947881, 2.999999999999999112 ) ) ;
#1431 = ITEM_DEFINED_TRANSFORMATION ( 'NONE', 'NONE', #10323,  #5704 ) ;
#1432 = CARTESIAN_POINT ( 'NONE',  ( 3.800000000000015365, 90.00000000000000000, 2.862500001229034474 ) ) ;
#1433 = ORIENTED_EDGE ( 'NONE', *, *, #9842, .F. ) ;
#1434 = DIRECTION ( 'NONE',  ( -0.8660254037844360431, -0.5000000000000047740, -0.000000000000000000 ) ) ;
#1435 = ADVANCED_FACE ( 'NONE', ( #9923 ), #7967, .T. ) ;
#1436 = VERTEX_POINT ( 'NONE', #10051 ) ;
#1437 = EDGE_CURVE ( 'NONE', #4511, #4278, #12939, .T. ) ;
#1438 = DIRECTION ( 'NONE',  ( -1.000000000000000000, 0.000000000000000000, 0.000000000000000000 ) ) ;
#1439 = ORIENTED_EDGE ( 'NONE', *, *, #2364, .F. ) ;
#1440 = FACE_BOUND ( 'NONE', #6999, .T. ) ;
#1441 = LINE ( 'NONE', #3416, #7058 ) ;
#1442 = SURFACE_STYLE_USAGE ( .BOTH. , #10276 ) ;
#1443 = AXIS2_PLACEMENT_3D ( 'NONE', #5383, #142, #7228 ) ;
#1444 = EDGE_CURVE ( 'NONE', #6695, #870, #3876, .T. ) ;
#1445 = VECTOR ( 'NONE', #1786, 1000.000000000000000 ) ;
#1446 = ORIENTED_EDGE ( 'NONE', *, *, #3128, .T. ) ;
#1447 = LINE ( 'NONE', #9429, #12008 ) ;
#1448 = ORIENTED_EDGE ( 'NONE', *, *, #3532, .F. ) ;
#1449 = LINE ( 'NONE', #9430, #6672 ) ;
#1450 = DIRECTION ( 'NONE',  ( -0.000000000000000000, 1.000000000000000000, -0.000000000000000000 ) ) ;
#1451 = PRODUCT ( 'socket button head screw_iso_ISO 7380 - M3 x 8 - 8N', 'socket button head screw_iso_ISO 7380 - M3 x 8 - 8N', '', ( #10334 ) ) ;
#1452 = ORIENTED_EDGE ( 'NONE', *, *, #2772, .T. ) ;
#1453 = VECTOR ( 'NONE', #6804, 1000.000000000000000 ) ;
#1454 = DIRECTION ( 'NONE',  ( 0.000000000000000000, 0.000000000000000000, -1.000000000000000000 ) ) ;
#1455 = CARTESIAN_POINT ( 'NONE',  ( 7.500000000000000000, 34.99999999999999289, 0.000000000000000000 ) ) ;
#1456 = CARTESIAN_POINT ( 'NONE',  ( 66.44356964374998142, 108.1539533981018053, 4.221875000614517148 ) ) ;
#1457 = CARTESIAN_POINT ( 'NONE',  ( 35.00000000000000000, 126.3079067962035822, 4.690625000614518036 ) ) ;
#1458 = ADVANCED_FACE ( 'NONE', ( #4045 ), #9800, .F. ) ;
#1459 = CARTESIAN_POINT ( 'NONE',  ( 2.387319993259524598, -4.036502139894371233, -0.8000000000000000444 ) ) ;
#1460 = CARTESIAN_POINT ( 'NONE',  ( 9.136132550659258555, 74.79933025939540414, -3.000000000000000000 ) ) ;
#1461 = CIRCLE ( 'NONE', #10650, 1.499999999999999556 ) ;
#1462 = DIRECTION ( 'NONE',  ( -0.000000000000000000, -0.000000000000000000, -1.000000000000000000 ) ) ;
#1463 = DIRECTION ( 'NONE',  ( -0.000000000000000000, 1.000000000000000000, -0.000000000000000000 ) ) ;
#1464 = CARTESIAN_POINT ( 'NONE',  ( 34.25000000000000000, 92.49999999999998579, -3.799999999999999378 ) ) ;
#1465 = FACE_OUTER_BOUND ( 'NONE', #4679, .T. ) ;
#1466 = ADVANCED_FACE ( 'NONE', ( #96 ), #3984, .F. ) ;
#1467 = DIRECTION ( 'NONE',  ( 1.000000000000000000, 0.000000000000000000, 0.000000000000000000 ) ) ;
#1468 = CARTESIAN_POINT ( 'NONE',  ( 40.00000000000000000, 0.000000000000000000, -1.499999999999999778 ) ) ;
#1469 = ORIENTED_EDGE ( 'NONE', *, *, #11376, .T. ) ;
#1470 = DIRECTION ( 'NONE',  ( -0.000000000000000000, 1.000000000000000000, -0.000000000000000000 ) ) ;
#1471 = DIRECTION ( 'NONE',  ( 0.000000000000000000, 0.000000000000000000, 1.000000000000000000 ) ) ;
#1472 = VERTEX_POINT ( 'NONE', #11949 ) ;
#1473 = EDGE_CURVE ( 'NONE', #443, #9678, #5994, .T. ) ;
#1474 = DIRECTION ( 'NONE',  ( 0.000000000000000000, -1.000000000000000000, 0.000000000000000000 ) ) ;
#1475 = DIRECTION ( 'NONE',  ( -0.000000000000000000, 1.000000000000000000, -0.000000000000000000 ) ) ;
#1476 = CARTESIAN_POINT ( 'NONE',  ( 66.19999999999988916, 71.98667160128361786, 4.737499999999998934 ) ) ;
#1477 = CARTESIAN_POINT ( 'NONE',  ( 35.49951382533862443, 118.9974510565036070, 4.000000000000000000 ) ) ;
#1478 = VECTOR ( 'NONE', #7745, 1000.000000000000000 ) ;
#1479 = VERTEX_POINT ( 'NONE', #830 ) ;
#1480 = LINE ( 'NONE', #2599, #10559 ) ;
#1481 = PLANE ( 'NONE',  #3567 ) ;
#1482 = VERTEX_POINT ( 'NONE', #4110 ) ;
#1483 = FILL_AREA_STYLE ('',( #6388 ) ) ;
#1484 = CARTESIAN_POINT ( 'NONE',  ( -53.33333333333332149, 33.84900179459755520, 1.000000000000000888 ) ) ;
#1485 = ORIENTED_EDGE ( 'NONE', *, *, #8450, .T. ) ;
#1486 = EDGE_CURVE ( 'NONE', #703, #11167, #3922, .T. ) ;
#1487 = DIRECTION ( 'NONE',  ( -0.3262398754384822630, 0.9452870165584014162, 0.000000000000000000 ) ) ;
#1488 = VERTEX_POINT ( 'NONE', #11030 ) ;
#1489 = EDGE_CURVE ( 'NONE', #191, #4989, #6156, .T. ) ;
#1490 = LINE ( 'NONE', #7512, #249 ) ;
#1491 = AXIS2_PLACEMENT_3D ( 'NONE', #12304, #2242, #3156 ) ;
#1492 = DIRECTION ( 'NONE',  ( 1.000000000000000000, 0.000000000000000000, 0.000000000000000000 ) ) ;
#1493 = EDGE_LOOP ( 'NONE', ( #12432, #9531 ) ) ;
#1494 =( BOUNDED_CURVE ( )  B_SPLINE_CURVE ( 2, ( #7440, #4369, #8360, #6386, #1415, #2473, #9461, #3522, #4498, #8491, #621, #12736, #4628, #5666, #3651, #813, #8616, #9719, #7631, #10828, #1807, #9784, #9656, #10766, #6774, #11683, #2668, #1872, #8803, #683, #4693, #12795, #3839, #3713, #4816, #7819, #2732, #752, #5793, #3776, #8739, #6643, #10638, #12607, #9595, #11815, #7757, #11747, #8679, #2862, #2793, #6835, #9847, #1680, #5857 ),
 .UNSPECIFIED., .F., .F. ) 
 B_SPLINE_CURVE_WITH_KNOTS ( ( 3, 2, 2, 2, 2, 2, 2, 2, 2, 2, 2, 2, 2, 2, 2, 2, 2, 2, 2, 2, 2, 2, 2, 2, 2, 2, 2, 3 ),
 ( 0.000000000000000000, 0.03333333333333333287, 0.06666666666666666574, 0.1000000000000000056, 0.1333333333333333315, 0.1666666666666666574, 0.2000000000000000111, 0.2333333333333333370, 0.2666666666666666630, 0.2999999999999999889, 0.3333333333333333148, 0.3666666666666666408, 0.4000000000000000222, 0.4333333333333333481, 0.4666666666666666741, 0.5000000000000000000, 0.5333333333333333259, 0.5666666666666666519, 0.5999999999999999778, 0.6333333333333333037, 0.6666666666666666297, 0.6999999999999999556, 0.7333333333333332815, 0.7666666666666667185, 0.8000000000000000444, 0.8333333333333333703, 0.8666666666666666963, 0.8887752010635167066 ),
 .UNSPECIFIED. ) 
 CURVE ( )  GEOMETRIC_REPRESENTATION_ITEM ( )  RATIONAL_B_SPLINE_CURVE ( ( 1.000000000000000000, 0.8660254037844387076, 1.000000000000000000, 0.8660254037844387076, 1.000000000000000000, 0.8660254037844387076, 1.000000000000000000, 0.8660254037844387076, 1.000000000000000000, 0.8660254037844387076, 1.000000000000000000, 0.8660254037844387076, 1.000000000000000000, 0.8660254037844387076, 1.000000000000000000, 0.8660254037844387076, 1.000000000000000000, 0.8660254037844387076, 1.000000000000000000, 0.8660254037844387076, 1.000000000000000000, 0.8660254037844387076, 1.000000000000000000, 0.8660254037844387076, 1.000000000000000000, 0.8660254037844387076, 1.000000000000000000, 0.8660254037844387076, 1.000000000000000000, 0.8660254037844387076, 1.000000000000000000, 0.8660254037844387076, 1.000000000000000000, 0.8660254037844387076, 1.000000000000000000, 0.8660254037844387076, 1.000000000000000000, 0.8660254037844387076, 1.000000000000000000, 0.8660254037844387076, 1.000000000000000000, 0.8660254037844387076, 1.000000000000000000, 0.8660254037844387076, 1.000000000000000000, 0.8660254037844387076, 1.000000000000000000, 0.8660254037844387076, 1.000000000000000000, 0.8660254037844387076, 1.000000000000000000, 0.8660254037844387076, 1.000000000000000000, 0.9111405409379251807, 0.9401542263054123438 ) ) 
 REPRESENTATION_ITEM ( '' )  );
#1495 = ORIENTED_EDGE ( 'NONE', *, *, #10898, .T. ) ;
#1496 = CARTESIAN_POINT ( 'NONE',  ( 21.49999999999998579, 90.00000000000000000, -8.000000000000000000 ) ) ;
#1497 = VERTEX_POINT ( 'NONE', #1822 ) ;
#1498 = LINE ( 'NONE', #8974, #7202 ) ;
#1499 = EDGE_LOOP ( 'NONE', ( #11671, #99, #12405, #1707, #12220, #9341 ) ) ;
#1500 = CIRCLE ( 'NONE', #661, 1.500000000000001332 ) ;
#1501 = CYLINDRICAL_SURFACE ( 'NONE', #12665, 4.999999999999997335 ) ;
#1502 = ORIENTED_EDGE ( 'NONE', *, *, #8330, .T. ) ;
#1503 = EDGE_CURVE ( 'NONE', #6072, #252, #4507, .T. ) ;
#1504 = FILL_AREA_STYLE ('',( #12569 ) ) ;
#1505 = ORIENTED_EDGE ( 'NONE', *, *, #9242, .T. ) ;
#1506 = CARTESIAN_POINT ( 'NONE',  ( 21.76320231625934554, 61.63142451696531765, 3.000000000000000000 ) ) ;
#1507 = CARTESIAN_POINT ( 'NONE',  ( -0.1698013801012111523, -5.473461295629626022, -0.8000000000000000444 ) ) ;
#1508 = AXIS2_PLACEMENT_3D ( 'NONE', #6409, #318, #11191 ) ;
#1510 = EDGE_CURVE ( 'NONE', #8482, #6635, #1285, .T. ) ;
#1509 = ORIENTED_EDGE ( 'NONE', *, *, #5837, .T. ) ;
#1511 = CARTESIAN_POINT ( 'NONE',  ( 3.556430356250015024, 90.00000000000000000, 3.509375000614517681 ) ) ;
#1512 = ORIENTED_EDGE ( 'NONE', *, *, #4521, .T. ) ;
#1513 = DIRECTION ( 'NONE',  ( 0.000000000000000000, -0.000000000000000000, -1.000000000000000000 ) ) ;
#1514 = EDGE_LOOP ( 'NONE', ( #2019, #3145, #9148, #1219 ) ) ;
#1515 = CARTESIAN_POINT ( 'NONE',  ( 3.556430356250028790, 71.84604660189818048, 4.446875000614517681 ) ) ;
#1516 = VERTEX_POINT ( 'NONE', #5340 ) ;
#1517 = LINE ( 'NONE', #4602, #4637 ) ;
#1518 = EDGE_CURVE ( 'NONE', #619, #8102, #2838, .T. ) ;
#1519 = CARTESIAN_POINT ( 'NONE',  ( 4.418411362812244114, 97.51822454362397252, 3.000000000000000444 ) ) ;
#1520 = CARTESIAN_POINT ( 'NONE',  ( 19.27821517812500574, 117.2309300971526937, 3.884375000614516793 ) ) ;
#1521 = CARTESIAN_POINT ( 'NONE',  ( 3.556430356250028790, 71.84604660189818048, 4.390625000614517326 ) ) ;
#1522 = DIRECTION ( 'NONE',  ( 0.9914448613738103822, -0.1305261922200528224, 0.000000000000000000 ) ) ;
#1523 = LINE ( 'NONE', #8338, #7931 ) ;
#1524 = EDGE_CURVE ( 'NONE', #8087, #11248, #2282, .T. ) ;
#1525 = LINE ( 'NONE', #2520, #1780 ) ;
#1526 = CARTESIAN_POINT ( 'NONE',  ( 66.19999999999998863, 90.00000000000000000, 3.087500001229034119 ) ) ;
#1527 = DIRECTION ( 'NONE',  ( 0.000000000000000000, 0.000000000000000000, -1.000000000000000000 ) ) ;
#1528 = VECTOR ( 'NONE', #12804, 1000.000000000000000 ) ;
#1529 = DIRECTION ( 'NONE',  ( 0.000000000000000000, 0.000000000000000000, 1.000000000000000000 ) ) ;
#1530 = CARTESIAN_POINT ( 'NONE',  ( 25.83484861008832567, 94.00000000000000000, -18.00000000000000355 ) ) ;
#1531 = CARTESIAN_POINT ( 'NONE',  ( -31.49999999999998579, 46.45448267190452896, 3.000000000000000000 ) ) ;
#1532 = ORIENTED_EDGE ( 'NONE', *, *, #4652, .F. ) ;
#1533 = CARTESIAN_POINT ( 'NONE',  ( 9.369499999999998607, 1.836970198721030181E-16, -1.500000000000000444 ) ) ;
#1534 = LINE ( 'NONE', #7429, #778 ) ;
#1535 = EDGE_LOOP ( 'NONE', ( #6310, #2117, #8009, #1866 ) ) ;
#1536 = CONICAL_SURFACE ( 'NONE', #6345, 1.499999999999999556, 1.029744259999998190 ) ;
#1537 = DIRECTION ( 'NONE',  ( -1.000000000000000000, 0.000000000000000000, 0.000000000000000000 ) ) ;
#1539 = CARTESIAN_POINT ( 'NONE',  ( 40.00000000000000000, 90.00000000000000000, -10.00000000000000000 ) ) ;
#1538 = PRODUCT_RELATED_PRODUCT_CATEGORY ( 'part', '', ( #2726 ) ) ;
#1540 = FACE_BOUND ( 'NONE', #3300, .T. ) ;
#1541 = AXIS2_PLACEMENT_3D ( 'NONE', #558, #8559, #5280 ) ;
#1542 = ORIENTED_EDGE ( 'NONE', *, *, #10710, .F. ) ;
#1543 = DIRECTION ( 'NONE',  ( 0.000000000000000000, 0.000000000000000000, 1.000000000000000000 ) ) ;
#1544 = EDGE_CURVE ( 'NONE', #3240, #4006, #11813, .T. ) ;
#1545 = DIRECTION ( 'NONE',  ( -0.9995191440486532741, -0.03100775193798452692, 0.000000000000000000 ) ) ;
#1546 = EDGE_LOOP ( 'NONE', ( #6390, #5719, #779, #12274, #2661 ) ) ;
#1547 = DIRECTION ( 'NONE',  ( 0.000000000000000000, 0.000000000000000000, 1.000000000000000000 ) ) ;
#1548 = AXIS2_PLACEMENT_3D ( 'NONE', #4416, #6432, #8603 ) ;
#1549 = DIRECTION ( 'NONE',  ( -1.000000000000000000, 0.000000000000000000, -0.000000000000000000 ) ) ;
#1550 = EDGE_LOOP ( 'NONE', ( #2996, #1028, #11226, #9089 ) ) ;
#1551 = VECTOR ( 'NONE', #10036, 1000.000000000000000 ) ;
#1552 = DIRECTION ( 'NONE',  ( 0.000000000000000000, -0.000000000000000000, 1.000000000000000000 ) ) ;
#1553 = ORIENTED_EDGE ( 'NONE', *, *, #8758, .T. ) ;
#1554 = DIRECTION ( 'NONE',  ( -0.000000000000000000, -0.000000000000000000, 1.000000000000000000 ) ) ;
#1555 = CARTESIAN_POINT ( 'NONE',  ( 6.499999999999999112, 65.10243346208218895, 2.999999999999960920 ) ) ;
#1556 = EDGE_LOOP ( 'NONE', ( #12315, #4021, #891, #11187 ) ) ;
#1557 = CARTESIAN_POINT ( 'NONE',  ( 66.19999999999998863, 90.00000000000000000, 4.325000000000000178 ) ) ;
#1558 = AXIS2_PLACEMENT_3D ( 'NONE', #12626, #10527, #2748 ) ;
#1559 = EDGE_CURVE ( 'NONE', #3514, #9678, #4177, .T. ) ;
#1560 = CARTESIAN_POINT ( 'NONE',  ( -36.66666666666665009, 2.000000000000000000, -7.999999999999996447 ) ) ;
#1561 = CIRCLE ( 'NONE', #8871, 1.000000000000000000 ) ;
#1562 = DIRECTION ( 'NONE',  ( 0.000000000000000000, 1.000000000000000000, 0.000000000000000000 ) ) ;
#1563 = ORIENTED_EDGE ( 'NONE', *, *, #9726, .T. ) ;
#1564 = CYLINDRICAL_SURFACE ( 'NONE', #12216, 4.338286831716297698 ) ;
#1565 = ADVANCED_FACE ( 'NONE', ( #420 ), #5276, .T. ) ;
#1566 = CARTESIAN_POINT ( 'NONE',  ( 66.20000000000000284, 71.98667160128370313, 3.950000001229034829 ) ) ;
#1567 = ORIENTED_EDGE ( 'NONE', *, *, #1605, .F. ) ;
#1568 = DIRECTION ( 'NONE',  ( -0.000000000000000000, -0.000000000000000000, -1.000000000000000000 ) ) ;
#1569 = VERTEX_POINT ( 'NONE', #12346 ) ;
#1570 = LINE ( 'NONE', #2625, #7138 ) ;
#1572 = ORIENTED_EDGE ( 'NONE', *, *, #5667, .F. ) ;
#1571 = AXIS2_PLACEMENT_3D ( 'NONE', #11421, #4561, #11488 ) ;
#1573 = VECTOR ( 'NONE', #371, 1000.000000000000000 ) ;
#1574 = DIRECTION ( 'NONE',  ( -0.000000000000000000, 1.000000000000000000, -0.000000000000000000 ) ) ;
#1575 = DIRECTION ( 'NONE',  ( 0.000000000000000000, -1.000000000000000000, 0.000000000000000000 ) ) ;
#1576 = EDGE_CURVE ( 'NONE', #3421, #5549, #7833, .T. ) ;
#1577 = ORIENTED_EDGE ( 'NONE', *, *, #9238, .F. ) ;
#1578 = CARTESIAN_POINT ( 'NONE',  ( 35.00000000000000000, 126.3079067962035822, 2.946875000614516793 ) ) ;
#1579 = ORIENTED_EDGE ( 'NONE', *, *, #11333, .T. ) ;
#1580 = AXIS2_PLACEMENT_3D ( 'NONE', #10565, #12391, #2459 ) ;
#1581 = CARTESIAN_POINT ( 'NONE',  ( 19.40000000000000924, 117.0199925980744666, 3.237500001229034030 ) ) ;
#1582 = AXIS2_PLACEMENT_3D ( 'NONE', #2816, #12754, #6984 ) ;
#1583 = ORIENTED_EDGE ( 'NONE', *, *, #4614, .T. ) ;
#1584 = CARTESIAN_POINT ( 'NONE',  ( 3.556430356250014579, 108.1539533981018053, 4.371875000614517504 ) ) ;
#1585 = VERTEX_POINT ( 'NONE', #8295 ) ;
#1586 = DIRECTION ( 'NONE',  ( -1.000000000000000000, -0.000000000000000000, -0.000000000000000000 ) ) ;
#1587 = LINE ( 'NONE', #7477, #8707 ) ;
#1588 = DIRECTION ( 'NONE',  ( 0.000000000000000000, -1.224646799147353207E-16, 1.000000000000000000 ) ) ;
#1589 = DIRECTION ( 'NONE',  ( -1.000000000000000000, -0.000000000000000000, -0.000000000000000000 ) ) ;
#1590 = APPLICATION_CONTEXT ( 'automotive_design' ) ;
#1591 = AXIS2_PLACEMENT_3D ( 'NONE', #9703, #4864, #1793 ) ;
#1592 = FACE_OUTER_BOUND ( 'NONE', #9632, .T. ) ;
#1593 = CIRCLE ( 'NONE', #8488, 30.00000000000000000 ) ;
#1594 = LINE ( 'NONE', #12326, #8142 ) ;
#1595 = EDGE_CURVE ( 'NONE', #191, #7314, #8165, .T. ) ;
#1596 = CYLINDRICAL_SURFACE ( 'NONE', #10760, 0.5999999999999998668 ) ;
#1597 = CARTESIAN_POINT ( 'NONE',  ( 64.99999999999998579, 122.5000000000001847, 1.000000000000003109 ) ) ;
#1598 = DIRECTION ( 'NONE',  ( -1.914177628664063178E-15, 1.000000000000000000, 0.000000000000000000 ) ) ;
#1599 = CARTESIAN_POINT ( 'NONE',  ( 1.040000000000000036, -0.5773502691896253980, -1.000000000000000000 ) ) ;
#1600 = VECTOR ( 'NONE', #11685, 1000.000000000000000 ) ;
#1601 = CARTESIAN_POINT ( 'NONE',  ( 36.50000000000001421, 79.80000000000001137, 6.000000000000000000 ) ) ;
#1602 = DIRECTION ( 'NONE',  ( 0.000000000000000000, 0.000000000000000000, -1.000000000000000000 ) ) ;
#1604 = ADVANCED_FACE ( 'NONE', ( #11357 ), #3197, .F. ) ;
#1603 = ORIENTED_EDGE ( 'NONE', *, *, #10158, .T. ) ;
#1605 = EDGE_CURVE ( 'NONE', #2737, #4447, #9508, .T. ) ;
#1606 = CARTESIAN_POINT ( 'NONE',  ( 19.40000000000000924, 117.0199925980744666, 4.474999999999999645 ) ) ;
#1607 = CARTESIAN_POINT ( 'NONE',  ( -6.666666666666660745, 2.000000000000000000, 1.599999999999992539 ) ) ;
#1608 = VERTEX_POINT ( 'NONE', #158 ) ;
#1609 =( NAMED_UNIT ( * ) PLANE_ANGLE_UNIT ( ) SI_UNIT ( $, .RADIAN. ) );
#1610 = AXIS2_PLACEMENT_3D ( 'NONE', #8427, #11560, #5610 ) ;
#1611 = CARTESIAN_POINT ( 'NONE',  ( -48.33333333333332860, 0.000000000000000000, 1.499999999999999556 ) ) ;
#1612 = CARTESIAN_POINT ( 'NONE',  ( 34.25000000000000000, 92.49999999999998579, -9.802775637731997449 ) ) ;
#1613 = VERTEX_POINT ( 'NONE', #3457 ) ;
#1614 = CARTESIAN_POINT ( 'NONE',  ( 3.800000000000015365, 90.00000000000000000, 4.212500001229034119 ) ) ;
#1615 = DIRECTION ( 'NONE',  ( 0.000000000000000000, 0.000000000000000000, -1.000000000000000000 ) ) ;
#1616 = ORIENTED_EDGE ( 'NONE', *, *, #8258, .F. ) ;
#1617 = LINE ( 'NONE', #1808, #7739 ) ;
#1618 = DIRECTION ( 'NONE',  ( -1.000000000000000000, 0.000000000000000000, 0.000000000000000000 ) ) ;
#1619 = ORIENTED_EDGE ( 'NONE', *, *, #12524, .T. ) ;
#1620 = CIRCLE ( 'NONE', #5170, 28.99999999999999289 ) ;
#1621 = DIRECTION ( 'NONE',  ( 1.049727191973305763E-16, 0.5150380737757249694, -0.8571673013836860200 ) ) ;
#1622 = ORIENTED_EDGE ( 'NONE', *, *, #5956, .T. ) ;
#1623 = PLANE ( 'NONE',  #1727 ) ;
#1624 = CARTESIAN_POINT ( 'NONE',  ( 32.09707732552327286, 88.32801317409231956, -3.800000000000000266 ) ) ;
#1625 = EDGE_CURVE ( 'NONE', #8631, #6452, #1357, .T. ) ;
#1626 = CARTESIAN_POINT ( 'NONE',  ( 3.800000000000015365, 90.00000000000000000, 4.549999999999999822 ) ) ;
#1627 = VERTEX_POINT ( 'NONE', #10313 ) ;
#1628 = CIRCLE ( 'NONE', #6230, 1.500000000000001332 ) ;
#1629 = DIRECTION ( 'NONE',  ( 0.000000000000000000, -1.000000000000000000, -0.000000000000000000 ) ) ;
#1630 = ORIENTED_EDGE ( 'NONE', *, *, #1964, .F. ) ;
#1631 = LINE ( 'NONE', #9737, #9293 ) ;
#1632 = CONTEXT_DEPENDENT_SHAPE_REPRESENTATION ( #2932, #11910 ) ;
#1633 = CARTESIAN_POINT ( 'NONE',  ( 3.800000000000025135, 71.98667160128366049, 3.800000001229034030 ) ) ;
#1634 = VERTEX_POINT ( 'NONE', #3268 ) ;
#1635 = FILL_AREA_STYLE ('',( #5557 ) ) ;
#1636 = VERTEX_POINT ( 'NONE', #3329 ) ;
#1637 = EDGE_CURVE ( 'NONE', #12207, #7597, #3676, .T. ) ;
#1638 = ORIENTED_EDGE ( 'NONE', *, *, #11170, .F. ) ;
#1639 = CIRCLE ( 'NONE', #4977, 1.499999999999999556 ) ;
#1640 = CARTESIAN_POINT ( 'NONE',  ( 3.535514453314946071, 90.20686785236708261, 2.999999999999999556 ) ) ;
#1641 = DIRECTION ( 'NONE',  ( -0.000000000000000000, -0.000000000000000000, -1.000000000000000000 ) ) ;
#1642 = EDGE_CURVE ( 'NONE', #8436, #4325, #12217, .T. ) ;
#1643 = UNCERTAINTY_MEASURE_WITH_UNIT (LENGTH_MEASURE( 1.000000000000000082E-05 ), #413, 'distance_accuracy_value', 'NONE');
#1644 = ORIENTED_EDGE ( 'NONE', *, *, #12182, .T. ) ;
#1645 = CARTESIAN_POINT ( 'NONE',  ( 66.19999999999998863, 90.00000000000000000, 4.437500001229033764 ) ) ;
#1646 = ORIENTED_EDGE ( 'NONE', *, *, #1230, .T. ) ;
#1647 = DIRECTION ( 'NONE',  ( 0.8090169943749456749, -0.5877852522924754686, 0.000000000000000000 ) ) ;
#1648 = ORIENTED_EDGE ( 'NONE', *, *, #1559, .T. ) ;
#1649 = CARTESIAN_POINT ( 'NONE',  ( 3.556430356250015024, 90.00000000000000000, 4.859375000614517326 ) ) ;
#1650 = EDGE_LOOP ( 'NONE', ( #2698, #765, #9307, #3005 ) ) ;
#1651 =( BOUNDED_CURVE ( )  B_SPLINE_CURVE ( 2, ( #8419, #4558, #5599, #618, #6704 ),
 .UNSPECIFIED., .F., .F. ) 
 B_SPLINE_CURVE_WITH_KNOTS ( ( 3, 2, 3 ),
 ( 0.7000000000000001776, 0.7333333333333332815, 0.7393280224290094127 ),
 .UNSPECIFIED. ) 
 CURVE ( )  GEOMETRIC_REPRESENTATION_ITEM ( )  RATIONAL_B_SPLINE_CURVE ( ( 0.9999999999999991118, 0.8660254037844395958, 1.000000000000000000, 0.9759059184690689337, 0.9604780286075660367 ) ) 
 REPRESENTATION_ITEM ( '' )  );
#1652 = CARTESIAN_POINT ( 'NONE',  ( -0.9999999999999997780, -4.273461295629625845, -0.8000000000000000444 ) ) ;
#1653 = CARTESIAN_POINT ( 'NONE',  ( 19.40000000000000924, 117.0199925980744666, 3.125000000000000000 ) ) ;
#1654 = EDGE_CURVE ( 'NONE', #1825, #11750, #10183, .T. ) ;
#1655 = DIRECTION ( 'NONE',  ( -1.000000000000000000, 0.000000000000000000, 0.000000000000000000 ) ) ;
#1656 = VECTOR ( 'NONE', #1725, 1000.000000000000000 ) ;
#1657 = FACE_OUTER_BOUND ( 'NONE', #4454, .T. ) ;
#1658 = AXIS2_PLACEMENT_3D ( 'NONE', #12179, #4204, #2310 ) ;
#1659 = LINE ( 'NONE', #5581, #3550 ) ;
#1660 = DIRECTION ( 'NONE',  ( -0.000000000000000000, 1.000000000000000000, -0.000000000000000000 ) ) ;
#1661 = LINE ( 'NONE', #6561, #5018 ) ;
#1662 = FACE_OUTER_BOUND ( 'NONE', #1514, .T. ) ;
#1663 = VECTOR ( 'NONE', #5897, 1000.000000000000000 ) ;
#1664 = DIRECTION ( 'NONE',  ( 0.9510565162951543083, -0.3090169943749451198, 0.000000000000000000 ) ) ;
#1665 = AXIS2_PLACEMENT_3D ( 'NONE', #9377, #9637, #4347 ) ;
#1666 = PLANE ( 'NONE',  #8597 ) ;
#1667 = DIRECTION ( 'NONE',  ( 0.000000000000000000, 0.000000000000000000, 1.000000000000000000 ) ) ;
#1668 = VERTEX_POINT ( 'NONE', #7174 ) ;
#1669 = ADVANCED_FACE ( 'NONE', ( #1348 ), #2217, .F. ) ;
#1670 = CARTESIAN_POINT ( 'NONE',  ( 35.00000000000000000, 126.0266567974326222, 4.437500000000000888 ) ) ;
#1671 = CARTESIAN_POINT ( 'NONE',  ( 8.499999999999998224, 66.25713400046146262, 1.000000000000000444 ) ) ;
#1672 = VERTEX_POINT ( 'NONE', #4242 ) ;
#1673 = AXIS2_PLACEMENT_3D ( 'NONE', #6725, #5686, #4896 ) ;
#1674 = DIRECTION ( 'NONE',  ( 0.000000000000000000, -1.000000000000000000, 1.370729058197317775E-18 ) ) ;
#1675 = EDGE_CURVE ( 'NONE', #7045, #4305, #3650, .T. ) ;
#1676 = DIRECTION ( 'NONE',  ( 0.000000000000000000, 0.000000000000000000, 1.000000000000000000 ) ) ;
#1677 = EDGE_CURVE ( 'NONE', #2240, #11707, #3586, .T. ) ;
#1678 = EDGE_LOOP ( 'NONE', ( #10019, #12881, #6928, #12253 ) ) ;
#1679 = CARTESIAN_POINT ( 'NONE',  ( 5.000000000000005329, 67.52776749732610995, -2.500000000000000000 ) ) ;
#1680 = CARTESIAN_POINT ( 'NONE',  ( 60.63303222545420823, 111.5086687406912347, 2.829484441871016109 ) ) ;
#1681 = VECTOR ( 'NONE', #5668, 1000.000000000000000 ) ;
#1682 = LINE ( 'NONE', #2863, #2317 ) ;
#1683 = CARTESIAN_POINT ( 'NONE',  ( 35.00000000000000000, 90.00000000000000000, -10.00000000000000000 ) ) ;
#1684 = EDGE_LOOP ( 'NONE', ( #9223, #1947 ) ) ;
#1685 = CARTESIAN_POINT ( 'NONE',  ( 20.00000000000000355, 2.000000000000000000, -10.00000000000000000 ) ) ;
#1686 = ORIENTED_EDGE ( 'NONE', *, *, #3091, .T. ) ;
#1687 = EDGE_CURVE ( 'NONE', #11451, #7582, #12014, .T. ) ;
#1688 = DIRECTION ( 'NONE',  ( 0.5877852522924715828, 0.8090169943749485615, 0.000000000000000000 ) ) ;
#1689 = DIRECTION ( 'NONE',  ( -5.624500927088228034E-17, 1.370729058197317968E-18, 1.000000000000000000 ) ) ;
#1690 = CIRCLE ( 'NONE', #3584, 30.19999999999999218 ) ;
#1691 = FACE_OUTER_BOUND ( 'NONE', #4404, .T. ) ;
#1692 = VERTEX_POINT ( 'NONE', #8490 ) ;
#1693 = CARTESIAN_POINT ( 'NONE',  ( -60.00000000000000000, 30.00000000000000000, 9.999999999999996447 ) ) ;
#1694 = VERTEX_POINT ( 'NONE', #4753 ) ;
#1695 = CARTESIAN_POINT ( 'NONE',  ( 9.999999999999994671, 76.58915998087155685, 2.500000000000000444 ) ) ;
#1696 = ITEM_DEFINED_TRANSFORMATION ( 'NONE', 'NONE', #2392,  #5704 ) ;
#1697 = DIRECTION ( 'NONE',  ( 0.000000000000000000, 1.000000000000000000, 0.000000000000000000 ) ) ;
#1698 = VERTEX_POINT ( 'NONE', #7439 ) ;
#1699 = EDGE_CURVE ( 'NONE', #8371, #11641, #8555, .T. ) ;
#1700 = CARTESIAN_POINT ( 'NONE',  ( 1.040000000000000036, -1.154700538379251684, -1.199226976249124676E-17 ) ) ;
#1701 = VERTEX_POINT ( 'NONE', #2472 ) ;
#1702 = VECTOR ( 'NONE', #1846, 1000.000000000000000 ) ;
#1703 = LINE ( 'NONE', #3735, #2331 ) ;
#1704 = ORIENTED_EDGE ( 'NONE', *, *, #2054, .F. ) ;
#1705 = CARTESIAN_POINT ( 'NONE',  ( 36.66058250612193348, 58.78194026151831508, 3.000000000000000000 ) ) ;
#1706 = DIRECTION ( 'NONE',  ( 0.000000000000000000, 0.000000000000000000, -1.000000000000000000 ) ) ;
#1707 = ORIENTED_EDGE ( 'NONE', *, *, #2445, .T. ) ;
#1708 = COLOUR_RGB ( '',1.000000000000000000, 0.9490196078431372140, 0.9098039215686274384 ) ;
#1709 = CARTESIAN_POINT ( 'NONE',  ( 30.00000000000000711, 2.000000000000000000, 10.00000000000000000 ) ) ;
#1710 = EDGE_CURVE ( 'NONE', #9206, #3826, #8877, .T. ) ;
#1711 = ORIENTED_EDGE ( 'NONE', *, *, #12047, .T. ) ;
#1712 = CARTESIAN_POINT ( 'NONE',  ( 34.25000000000000000, 93.41869858279433458, 4.000000000000000000 ) ) ;
#1713 = EDGE_LOOP ( 'NONE', ( #9085, #4380, #10994, #12223 ) ) ;
#1714 = CARTESIAN_POINT ( 'NONE',  ( 66.44356964374999563, 71.84604660189820891, 3.190625000614517592 ) ) ;
#1715 = ADVANCED_FACE ( 'NONE', ( #5601 ), #9718, .F. ) ;
#1716 = ORIENTED_EDGE ( 'NONE', *, *, #988, .T. ) ;
#1717 = CARTESIAN_POINT ( 'NONE',  ( 66.19999999999998863, 90.00000000000000000, 3.875000000000000000 ) ) ;
#1718 = LINE ( 'NONE', #5706, #4125 ) ;
#1719 = DIRECTION ( 'NONE',  ( -0.000000000000000000, 1.000000000000000000, -0.000000000000000000 ) ) ;
#1720 = AXIS2_PLACEMENT_3D ( 'NONE', #10273, #10210, #7396 ) ;
#1721 = CARTESIAN_POINT ( 'NONE',  ( 35.00000000000000711, 53.69209320379640360, 4.015625000614517326 ) ) ;
#1722 = DIRECTION ( 'NONE',  ( 0.000000000000000000, -0.000000000000000000, -1.000000000000000000 ) ) ;
#1723 = CYLINDRICAL_SURFACE ( 'NONE', #4906, 31.19999999999999929 ) ;
#1724 = EDGE_CURVE ( 'NONE', #6762, #12412, #3252, .T. ) ;
#1725 = DIRECTION ( 'NONE',  ( -0.000000000000000000, -0.000000000000000000, -1.000000000000000000 ) ) ;
#1726 = CARTESIAN_POINT ( 'NONE',  ( 18.35873618070580093, 66.24461453698026503, 2.333333333333333481 ) ) ;
#1727 = AXIS2_PLACEMENT_3D ( 'NONE', #9605, #10958, #1815 ) ;
#1728 = CARTESIAN_POINT ( 'NONE',  ( 3.800000000000015365, 90.00000000000000000, 4.831250000614517148 ) ) ;
#1729 = EDGE_CURVE ( 'NONE', #3927, #7180, #732, .T. ) ;
#1730 = CARTESIAN_POINT ( 'NONE',  ( 33.50000000000000711, 79.80000000000001137, 8.000000000000000000 ) ) ;
#1731 = CARTESIAN_POINT ( 'NONE',  ( 19.27821517812503060, 62.76906990284727783, 3.134375000614517237 ) ) ;
#1732 = EDGE_LOOP ( 'NONE', ( #4996, #3921, #6198 ) ) ;
#1733 = CARTESIAN_POINT ( 'NONE',  ( 50.59999999999999432, 117.0199925980744666, 3.050000000000000266 ) ) ;
#1734 = DIRECTION ( 'NONE',  ( 0.1305261922200528224, -0.9914448613738103822, 0.000000000000000000 ) ) ;
#1735 = VERTEX_POINT ( 'NONE', #3711 ) ;
#1736 = SURFACE_STYLE_FILL_AREA ( #6151 ) ;
#1737 = DIRECTION ( 'NONE',  ( -0.000000000000000000, -0.000000000000000000, -1.000000000000000000 ) ) ;
#1738 = EDGE_CURVE ( 'NONE', #4892, #12446, #1480, .T. ) ;
#1739 = CARTESIAN_POINT ( 'NONE',  ( 45.00000000000000000, 2.000000000000000000, 4.150000000000006573 ) ) ;
#1740 = DIRECTION ( 'NONE',  ( 1.000000000000000000, 0.000000000000000000, 0.000000000000000000 ) ) ;
#1741 = CARTESIAN_POINT ( 'NONE',  ( 45.00000000000000000, 0.000000000000000000, 5.750000000000000888 ) ) ;
#1742 = LINE ( 'NONE', #5730, #2308 ) ;
#1743 = CARTESIAN_POINT ( 'NONE',  ( 35.00000000000000000, 126.3079067962036106, 4.296875000614517326 ) ) ;
#1744 = VERTEX_POINT ( 'NONE', #9459 ) ;
#1745 = CARTESIAN_POINT ( 'NONE',  ( 5.904717470405908664, 81.90651283295660789, 5.000000000000000000 ) ) ;
#1746 = EDGE_LOOP ( 'NONE', ( #9745, #2949, #5116, #2908, #10024, #12272 ) ) ;
#1747 = AXIS2_PLACEMENT_3D ( 'NONE', #4106, #7242, #4302 ) ;
#1748 = CYLINDRICAL_SURFACE ( 'NONE', #6951, 28.99999999999999289 ) ;
#1749 = DIRECTION ( 'NONE',  ( -1.000000000000000000, -0.000000000000000000, -0.000000000000000000 ) ) ;
#1750 = CARTESIAN_POINT ( 'NONE',  ( 35.00000000000000000, 90.00000000000000000, 22.38477631085024555 ) ) ;
#1751 = LINE ( 'NONE', #9733, #1528 ) ;
#1752 = CARTESIAN_POINT ( 'NONE',  ( 1.269999999999999796, 0.000000000000000000, 0.000000000000000000 ) ) ;
#1753 = CARTESIAN_POINT ( 'NONE',  ( 1.269999999999999796, 0.000000000000000000, 0.000000000000000000 ) ) ;
#1754 = ORIENTED_EDGE ( 'NONE', *, *, #5511, .F. ) ;
#1755 = VECTOR ( 'NONE', #9529, 1000.000000000000000 ) ;
#1756 = CYLINDRICAL_SURFACE ( 'NONE', #9711, 31.19999999999998863 ) ;
#1757 = DIRECTION ( 'NONE',  ( -0.000000000000000000, -0.000000000000000000, -1.000000000000000000 ) ) ;
#1758 = AXIS2_PLACEMENT_3D ( 'NONE', #7951, #4813, #9843 ) ;
#1759 = ORIENTED_EDGE ( 'NONE', *, *, #6632, .F. ) ;
#1760 = CARTESIAN_POINT ( 'NONE',  ( -0.1698013801012111523, -5.473461295629626022, -0.8000000000000000444 ) ) ;
#1761 = ORIENTED_EDGE ( 'NONE', *, *, #2695, .T. ) ;
#1762 = PRODUCT_DEFINITION_FORMATION_WITH_SPECIFIED_SOURCE ( 'ANY', '', #11480, .NOT_KNOWN. ) ;
#1763 = CARTESIAN_POINT ( 'NONE',  ( 1.649999999999999911, 0.000000000000000000, 2.849999999999999645 ) ) ;
#1764 = ORIENTED_EDGE ( 'NONE', *, *, #2695, .F. ) ;
#1765 = EDGE_CURVE ( 'NONE', #9740, #3991, #8262, .T. ) ;
#1766 = EDGE_CURVE ( 'NONE', #8153, #11802, #9655, .T. ) ;
#1767 = CARTESIAN_POINT ( 'NONE',  ( 35.00000000000000000, 90.00000000000000000, -3.000000000000000000 ) ) ;
#1768 = DIRECTION ( 'NONE',  ( -0.8660254037844394848, -0.4999999999999984457, -0.000000000000000000 ) ) ;
#1769 = AXIS2_PLACEMENT_3D ( 'NONE', #403, #2652, #8472 ) ;
#1770 = VECTOR ( 'NONE', #1737, 1000.000000000000000 ) ;
#1771 = ORIENTED_EDGE ( 'NONE', *, *, #9226, .T. ) ;
#1772 = FACE_OUTER_BOUND ( 'NONE', #2765, .T. ) ;
#1773 = EDGE_LOOP ( 'NONE', ( #4370, #8040, #4865, #4151 ) ) ;
#1774 = DIRECTION ( 'NONE',  ( -0.3262398754384820410, 0.9452870165584015272, 0.000000000000000000 ) ) ;
#1775 = EDGE_LOOP ( 'NONE', ( #3619, #4581, #9169, #3707 ) ) ;
#1776 = AXIS2_PLACEMENT_3D ( 'NONE', #10333, #3167, #2182 ) ;
#1777 = DIRECTION ( 'NONE',  ( -0.000000000000000000, -0.000000000000000000, -1.000000000000000000 ) ) ;
#1778 = PRODUCT_DEFINITION_SHAPE ( 'NONE', 'NONE',  #12970 ) ;
#1779 = VERTEX_POINT ( 'NONE', #1614 ) ;
#1780 = VECTOR ( 'NONE', #5516, 1000.000000000000227 ) ;
#1781 = DIRECTION ( 'NONE',  ( 1.000000000000000000, 0.000000000000000000, 0.000000000000000000 ) ) ;
#1782 = DIRECTION ( 'NONE',  ( 0.000000000000000000, 0.000000000000000000, 1.000000000000000000 ) ) ;
#1783 = DIRECTION ( 'NONE',  ( 0.000000000000000000, 0.000000000000000000, 1.000000000000000000 ) ) ;
#1784 = CARTESIAN_POINT ( 'NONE',  ( 3.800000000000015365, 90.00000000000000000, 4.212500001229034119 ) ) ;
#1785 = VECTOR ( 'NONE', #1740, 1000.000000000000000 ) ;
#1786 = DIRECTION ( 'NONE',  ( -0.000000000000000000, -1.000000000000000000, -0.000000000000000000 ) ) ;
#1787 = ADVANCED_FACE ( 'NONE', ( #9594 ), #620, .T. ) ;
#1788 = CARTESIAN_POINT ( 'NONE',  ( -67.46410161513773573, 36.92820323027551410, -2.500000000000000000 ) ) ;
#1789 = VECTOR ( 'NONE', #4577, 1000.000000000000000 ) ;
#1790 = CARTESIAN_POINT ( 'NONE',  ( 65.19999999999998863, 90.00000000000000000, 5.000000000000000000 ) ) ;
#1791 = FACE_BOUND ( 'NONE', #2135, .T. ) ;
#1792 = CARTESIAN_POINT ( 'NONE',  ( 39.21379230364325252, 85.05086326499692007, 4.000000000000000000 ) ) ;
#1793 = DIRECTION ( 'NONE',  ( -1.000000000000000000, 0.000000000000000000, 0.000000000000000000 ) ) ;
#1794 = CARTESIAN_POINT ( 'NONE',  ( 5.000000000000004441, 30.00000000000000000, 2.500000000000000444 ) ) ;
#1795 = VECTOR ( 'NONE', #209, 1000.000000000000000 ) ;
#1796 = CARTESIAN_POINT ( 'NONE',  ( 19.27821517812500574, 117.2309300971526937, 4.334375000614516971 ) ) ;
#1797 = ORIENTED_EDGE ( 'NONE', *, *, #731, .T. ) ;
#1798 = CARTESIAN_POINT ( 'NONE',  ( 66.19999999999997442, 108.0133283987163253, 4.812500000000000000 ) ) ;
#1799 = EDGE_CURVE ( 'NONE', #4047, #2314, #7503, .T. ) ;
#1800 = DIRECTION ( 'NONE',  ( 1.000000000000000000, 0.000000000000000000, -0.000000000000000000 ) ) ;
#1801 = EDGE_LOOP ( 'NONE', ( #4383, #257 ) ) ;
#1802 = ADVANCED_FACE ( 'NONE', ( #9532 ), #12606, .F. ) ;
#1803 = EDGE_CURVE ( 'NONE', #4911, #5204, #10636, .T. ) ;
#1804 = CYLINDRICAL_SURFACE ( 'NONE', #11999, 32.70000000000000284 ) ;
#1805 = DIRECTION ( 'NONE',  ( 1.000000000000000000, 0.000000000000000000, 0.000000000000000000 ) ) ;
#1806 = PLANE ( 'NONE',  #1370 ) ;
#1807 = CARTESIAN_POINT ( 'NONE',  ( 50.72178482187501203, 62.76906990284730625, 4.053125000614517859 ) ) ;
#1808 = CARTESIAN_POINT ( 'NONE',  ( -28.99038105676692112, 50.21281292110204930, -1.000000000000000000 ) ) ;
#1809 = DIRECTION ( 'NONE',  ( 1.000000000000000000, 0.000000000000000000, -0.000000000000000000 ) ) ;
#1810 = VERTEX_POINT ( 'NONE', #1679 ) ;
#1811 = DIRECTION ( 'NONE',  ( -1.000000000000000000, 0.000000000000000000, 0.000000000000000000 ) ) ;
#1812 = ORIENTED_EDGE ( 'NONE', *, *, #2129, .T. ) ;
#1813 = EDGE_CURVE ( 'NONE', #835, #10173, #10698, .T. ) ;
#1814 = AXIS2_PLACEMENT_3D ( 'NONE', #4355, #4548, #12595 ) ;
#1815 = DIRECTION ( 'NONE',  ( -0.8660254037844361541, -0.5000000000000042188, 0.000000000000000000 ) ) ;
#1816 = DIRECTION ( 'NONE',  ( -5.624500927088228034E-17, 1.370729058197317775E-18, 1.000000000000000000 ) ) ;
#1817 = CARTESIAN_POINT ( 'NONE',  ( 35.00000000000000000, 90.00000000000000000, 4.000000000000000000 ) ) ;
#1818 = CARTESIAN_POINT ( 'NONE',  ( 20.00000000000000355, 2.000000000000000000, 10.00000000000000000 ) ) ;
#1819 = DIRECTION ( 'NONE',  ( 0.8660254037844361541, 0.5000000000000042188, 0.000000000000000000 ) ) ;
#1820 = DIRECTION ( 'NONE',  ( -2.891205793294679312E-17, -0.000000000000000000, 1.000000000000000000 ) ) ;
#1821 = VERTEX_POINT ( 'NONE', #6707 ) ;
#1822 = CARTESIAN_POINT ( 'NONE',  ( 44.20597631976078645, 117.5000000000000568, -0.9999999999999974465 ) ) ;
#1823 = DIRECTION ( 'NONE',  ( 0.000000000000000000, 0.000000000000000000, 1.000000000000000000 ) ) ;
#1824 = VECTOR ( 'NONE', #494, 1000.000000000000000 ) ;
#1825 = VERTEX_POINT ( 'NONE', #751 ) ;
#1826 = B_SPLINE_CURVE_WITH_KNOTS ( 'NONE', 3,
 ( #8864, #11935, #9844, #3836 ),
 .UNSPECIFIED., .F., .F.,
 ( 4, 4 ),
 ( 0.000000000000000000, 1.000000000000000000 ),
 .UNSPECIFIED. ) ;
#1827 = FACE_OUTER_BOUND ( 'NONE', #289, .T. ) ;
#1828 = ORIENTED_EDGE ( 'NONE', *, *, #4046, .T. ) ;
#1829 = DIRECTION ( 'NONE',  ( -0.5000000000000043299, 0.8660254037844362651, 0.000000000000000000 ) ) ;
#1830 = VERTEX_POINT ( 'NONE', #5004 ) ;
#1831 = EDGE_CURVE ( 'NONE', #6585, #11492, #9090, .T. ) ;
#1832 = DIRECTION ( 'NONE',  ( 0.000000000000000000, 0.000000000000000000, 1.000000000000000000 ) ) ;
#1833 = FACE_OUTER_BOUND ( 'NONE', #10045, .T. ) ;
#1834 = VECTOR ( 'NONE', #5391, 1000.000000000000000 ) ;
#1835 = ORIENTED_EDGE ( 'NONE', *, *, #11333, .F. ) ;
#1836 = CARTESIAN_POINT ( 'NONE',  ( 25.00000000000000355, -5.000000000000000000, 4.249999999999998224 ) ) ;
#1837 = EDGE_LOOP ( 'NONE', ( #829, #11058 ) ) ;
#1838 = APPLICATION_CONTEXT ( 'automotive_design' ) ;
#1839 = EDGE_CURVE ( 'NONE', #12641, #8130, #11823, .T. ) ;
#1840 = CARTESIAN_POINT ( 'NONE',  ( 1.269999999999999796, 0.000000000000000000, 0.000000000000000000 ) ) ;
#1841 = EDGE_CURVE ( 'NONE', #6922, #6635, #12237, .T. ) ;
#1842 = ORIENTED_EDGE ( 'NONE', *, *, #9583, .T. ) ;
#1843 = CARTESIAN_POINT ( 'NONE',  ( 50.72178482187499071, 117.2309300971526937, 3.753125000614517592 ) ) ;
#1844 = ORIENTED_EDGE ( 'NONE', *, *, #11101, .F. ) ;
#1845 = VECTOR ( 'NONE', #3309, 999.9999999999998863 ) ;
#1846 = DIRECTION ( 'NONE',  ( -0.000000000000000000, 1.000000000000000000, -0.000000000000000000 ) ) ;
#1847 = DIRECTION ( 'NONE',  ( -0.000000000000000000, -1.000000000000000000, -0.000000000000000000 ) ) ;
#1848 = CARTESIAN_POINT ( 'NONE',  ( 25.00000000000000355, 2.000000000000001332, 5.750000000000000000 ) ) ;
#1849 = CARTESIAN_POINT ( 'NONE',  ( 19.40000000000002700, 62.98000740192551206, 3.837500001229034563 ) ) ;
#1850 = ADVANCED_FACE ( 'NONE', ( #8989 ), #5792, .F. ) ;
#1851 = CARTESIAN_POINT ( 'NONE',  ( 33.50000000000000711, 67.79999999999999716, 8.000000000000000000 ) ) ;
#1852 = AXIS2_PLACEMENT_3D ( 'NONE', #1555, #303, #7378 ) ;
#1853 = CARTESIAN_POINT ( 'NONE',  ( 43.71630314554308683, 62.34089554097972297, 4.000000000000000000 ) ) ;
#1854 = CARTESIAN_POINT ( 'NONE',  ( 1.000000000000000000, -5.473461295629626022, -0.8000000000000000444 ) ) ;
#1855 = CARTESIAN_POINT ( 'NONE',  ( 51.63879093662676922, 66.24814457421848601, 3.000000000000000888 ) ) ;
#1856 = DIRECTION ( 'NONE',  ( 0.000000000000000000, 0.000000000000000000, 1.000000000000000000 ) ) ;
#1857 = CARTESIAN_POINT ( 'NONE',  ( 13.22666678878058200, 110.6378768499380527, 1.000000000000003553 ) ) ;
#1858 = ORIENTED_EDGE ( 'NONE', *, *, #10378, .T. ) ;
#1859 = LINE ( 'NONE', #5846, #2536 ) ;
#1860 = CARTESIAN_POINT ( 'NONE',  ( 19.27821517812503060, 62.76906990284727783, 4.484375000614516438 ) ) ;
#1861 = EDGE_CURVE ( 'NONE', #6806, #1692, #2861, .T. ) ;
#1862 = VERTEX_POINT ( 'NONE', #11 ) ;
#1863 = AXIS2_PLACEMENT_3D ( 'NONE', #4323, #6337, #7327 ) ;
#1864 = CARTESIAN_POINT ( 'NONE',  ( 3.800000000000015365, 90.00000000000000000, 3.650000000000000355 ) ) ;
#1865 = FACE_OUTER_BOUND ( 'NONE', #5143, .T. ) ;
#1866 = ORIENTED_EDGE ( 'NONE', *, *, #1004, .F. ) ;
#1867 = AXIS2_PLACEMENT_3D ( 'NONE', #7290, #11337, #207 ) ;
#1868 = CARTESIAN_POINT ( 'NONE',  ( 34.50001867552290946, 118.9978264099154615, 4.000000000000000000 ) ) ;
#1869 = CARTESIAN_POINT ( 'NONE',  ( 35.00000000000000000, 90.00000000000000000, 1.000000000000003553 ) ) ;
#1870 = CIRCLE ( 'NONE', #9177, 3.350000000000003642 ) ;
#1871 = LINE ( 'NONE', #6773, #5335 ) ;
#1872 = CARTESIAN_POINT ( 'NONE',  ( 35.00000000000000000, 126.3079067962036106, 3.790625000614517237 ) ) ;
#1873 = LINE ( 'NONE', #7698, #1681 ) ;
#1874 = CARTESIAN_POINT ( 'NONE',  ( 66.44356964374999563, 90.00000000000000000, 4.634375000614516793 ) ) ;
#1875 = EDGE_CURVE ( 'NONE', #10645, #1694, #6587, .T. ) ;
#1876 = ORIENTED_EDGE ( 'NONE', *, *, #8811, .T. ) ;
#1877 = VECTOR ( 'NONE', #11062, 1000.000000000000000 ) ;
#1878 = FACE_OUTER_BOUND ( 'NONE', #11584, .T. ) ;
#1879 = EDGE_LOOP ( 'NONE', ( #11841, #12494, #1646, #4523 ) ) ;
#1880 = DIRECTION ( 'NONE',  ( 0.4999999999999995559, -0.8660254037844389297, 0.000000000000000000 ) ) ;
#1881 = FACE_OUTER_BOUND ( 'NONE', #9933, .T. ) ;
#1882 = CARTESIAN_POINT ( 'NONE',  ( 38.50000000000000711, 90.00000000000000000, 4.000000000000000000 ) ) ;
#1884 = DIRECTION ( 'NONE',  ( -1.000000000000000000, -0.000000000000000000, -0.000000000000000000 ) ) ;
#1883 = CIRCLE ( 'NONE', #2727, 4.000000000000000000 ) ;
#1885 = ORIENTED_EDGE ( 'NONE', *, *, #2003, .F. ) ;
#1886 = CARTESIAN_POINT ( 'NONE',  ( 45.00000000000000000, -5.000000000000000000, -4.249999999999998224 ) ) ;
#1887 = DIRECTION ( 'NONE',  ( 0.000000000000000000, 0.000000000000000000, 1.000000000000000000 ) ) ;
#1888 = EDGE_CURVE ( 'NONE', #408, #2123, #103, .T. ) ;
#1889 = ORIENTED_EDGE ( 'NONE', *, *, #9910, .T. ) ;
#1890 = LINE ( 'NONE', #9865, #5546 ) ;
#1891 = EDGE_CURVE ( 'NONE', #7660, #1613, #7888, .T. ) ;
#1892 = VERTEX_POINT ( 'NONE', #2065 ) ;
#1893 = DIRECTION ( 'NONE',  ( -1.000000000000000000, -3.349810850162111054E-15, 0.000000000000000000 ) ) ;
#1894 = VERTEX_POINT ( 'NONE', #8017 ) ;
#1895 = CARTESIAN_POINT ( 'NONE',  ( -0.2000000000000000111, -6.446898479113814417, -0.8000000000000000444 ) ) ;
#1896 = AXIS2_PLACEMENT_3D ( 'NONE', #6709, #8681, #753 ) ;
#1897 = CARTESIAN_POINT ( 'NONE',  ( 66.19999999999998863, 90.00000000000000000, 3.425000000000000266 ) ) ;
#1898 = VERTEX_POINT ( 'NONE', #6834 ) ;
#1899 = DIRECTION ( 'NONE',  ( -1.000000000000000000, 0.000000000000000000, 0.000000000000000000 ) ) ;
#1900 = ORIENTED_EDGE ( 'NONE', *, *, #7233, .F. ) ;
#1901 = CARTESIAN_POINT ( 'NONE',  ( 1.000000000000000000, -5.473461295629626022, -0.8000000000000000444 ) ) ;
#1902 = EDGE_CURVE ( 'NONE', #8617, #4915, #313, .T. ) ;
#1903 = ORIENTED_EDGE ( 'NONE', *, *, #8109, .F. ) ;
#1904 = AXIS2_PLACEMENT_3D ( 'NONE', #12320, #3368, #6359 ) ;
#1905 = CARTESIAN_POINT ( 'NONE',  ( 35.00000000000000711, 53.69209320379640360, 4.015625000614517326 ) ) ;
#1906 = VERTEX_POINT ( 'NONE', #9783 ) ;
#1907 = DIRECTION ( 'NONE',  ( -1.000000000000000000, -0.000000000000000000, -0.000000000000000000 ) ) ;
#1908 = LINE ( 'NONE', #659, #6411 ) ;
#1909 = CARTESIAN_POINT ( 'NONE',  ( 3.800000000000025580, 71.98667160128366049, 3.350000001229034297 ) ) ;
#1910 = CARTESIAN_POINT ( 'NONE',  ( 19.27821517812500574, 117.2309300971526937, 3.828125000614516882 ) ) ;
#1911 = EDGE_CURVE ( 'NONE', #6195, #5352, #1871, .T. ) ;
#1912 = VECTOR ( 'NONE', #5237, 1000.000000000000114 ) ;
#1913 = CARTESIAN_POINT ( 'NONE',  ( 35.00000000000000000, 90.00000000000000000, 5.000000000000000000 ) ) ;
#1914 = ORIENTED_EDGE ( 'NONE', *, *, #8639, .T. ) ;
#1915 =( BOUNDED_CURVE ( )  B_SPLINE_CURVE ( 2, ( #1368, #4386, #7387, #5484, #9550, #9414, #574 ),
 .UNSPECIFIED., .F., .F. ) 
 B_SPLINE_CURVE_WITH_KNOTS ( ( 3, 2, 2, 3 ),
 ( 0.7000000000000001776, 0.7333333333333335036, 0.7666666666666669405, 0.8000000000000002665 ),
 .UNSPECIFIED. ) 
 CURVE ( )  GEOMETRIC_REPRESENTATION_ITEM ( )  RATIONAL_B_SPLINE_CURVE ( ( 0.9999999999999991118, 0.8660254037844395958, 1.000000000000000000, 0.8660254037844387076, 1.000000000000000000, 0.8660254037844378194, 1.000000000000000888 ) ) 
 REPRESENTATION_ITEM ( '' )  );
#1916 = DIRECTION ( 'NONE',  ( -1.000000000000000000, -0.000000000000000000, -0.000000000000000000 ) ) ;
#1917 = CARTESIAN_POINT ( 'NONE',  ( -43.33333333333332860, 39.62250448649387380, 3.000000000000000000 ) ) ;
#1918 = CARTESIAN_POINT ( 'NONE',  ( 14.50114310663104966, 113.8451850114809361, 2.999999999999999112 ) ) ;
#1919 = EDGE_LOOP ( 'NONE', ( #1358, #1009, #9756, #4335 ) ) ;
#1920 = FACE_OUTER_BOUND ( 'NONE', #12041, .T. ) ;
#1921 = ORIENTED_EDGE ( 'NONE', *, *, #8275, .F. ) ;
#1922 = MECHANICAL_DESIGN_GEOMETRIC_PRESENTATION_REPRESENTATION (  '', ( #11529 ), #10056 ) ;
#1923 = CARTESIAN_POINT ( 'NONE',  ( 37.99038105676688559, 21.93375672974103452, -1.000000000000000000 ) ) ;
#1924 = CARTESIAN_POINT ( 'NONE',  ( 50.72178482187501203, 62.76906990284730625, 3.209375000614517415 ) ) ;
#1925 = EDGE_LOOP ( 'NONE', ( #8389, #9356, #4884, #1317 ) ) ;
#1926 = CARTESIAN_POINT ( 'NONE',  ( 50.72178482187499071, 117.2309300971526937, 2.909375000614517148 ) ) ;
#1927 = CARTESIAN_POINT ( 'NONE',  ( 66.19999999999998863, 90.00000000000000000, 4.774999999999999467 ) ) ;
#1928 = ADVANCED_FACE ( 'NONE', ( #8928 ), #1806, .F. ) ;
#1929 = EDGE_CURVE ( 'NONE', #6997, #4594, #6945, .T. ) ;
#1930=STYLED_ITEM('',(#13002),#12156);
#1931 = CARTESIAN_POINT ( 'NONE',  ( 35.00000000000000000, 90.00000000000000000, 1.000000000000003553 ) ) ;
#1932 = CARTESIAN_POINT ( 'NONE',  ( -18.33333333333332504, 2.000000000000000000, -8.000000000000001776 ) ) ;
#1933 = DIRECTION ( 'NONE',  ( 0.000000000000000000, -1.000000000000000000, 0.000000000000000000 ) ) ;
#1934 = CARTESIAN_POINT ( 'NONE',  ( 0.000000000000000000, 0.000000000000000000, 2.500000000000000000 ) ) ;
#1935 = CARTESIAN_POINT ( 'NONE',  ( 66.44356964374998142, 108.1539533981018053, 4.671875000614517326 ) ) ;
#1936 = ORIENTED_EDGE ( 'NONE', *, *, #8160, .F. ) ;
#1937 = AXIS2_PLACEMENT_3D ( 'NONE', #12487, #3661, #12617 ) ;
#1938 = DIRECTION ( 'NONE',  ( -1.000000000000000000, -0.000000000000000000, -0.000000000000000000 ) ) ;
#1939 = VERTEX_POINT ( 'NONE', #11814 ) ;
#1940 = LINE ( 'NONE', #9981, #49 ) ;
#1941 = CARTESIAN_POINT ( 'NONE',  ( 66.20000000000008811, 108.0133283987162542, 3.462499999999999467 ) ) ;
#1942 = CARTESIAN_POINT ( 'NONE',  ( 45.00000000000000000, 0.000000000000000000, -4.150000000000003020 ) ) ;
#1943 = ADVANCED_FACE ( 'NONE', ( #7953 ), #12793, .F. ) ;
#1944 = CARTESIAN_POINT ( 'NONE',  ( 1.040000000000000036, 1.154700538379252350, -1.084202172485497162E-16 ) ) ;
#1945 = STYLED_ITEM ( 'NONE', ( #9062 ), #2170 ) ;
#1946 = DIRECTION ( 'NONE',  ( -0.8660254037844365982, -0.5000000000000036637, 0.000000000000000000 ) ) ;
#1947 = ORIENTED_EDGE ( 'NONE', *, *, #9870, .T. ) ;
#1948 = CARTESIAN_POINT ( 'NONE',  ( 4.999999999999962697, 79.07477288111861924, 3.000000000000000000 ) ) ;
#1949 = CARTESIAN_POINT ( 'NONE',  ( 30.00000000000000711, 121.2009999999999934, 1.500000000000000666 ) ) ;
#1950 = ORIENTED_EDGE ( 'NONE', *, *, #9238, .T. ) ;
#1951 = CLOSED_SHELL ( 'NONE', ( #2139, #6471, #593, #3644, #3730, #1928, #5531, #338, #6814, #6013, #11811, #954, #12893, #7708, #287 ) ) ;
#1952 =( LENGTH_UNIT ( ) NAMED_UNIT ( * ) SI_UNIT ( .MILLI., .METRE. ) );
#1953 = AXIS2_PLACEMENT_3D ( 'NONE', #2238, #4065, #6012 ) ;
#1954 = LINE ( 'NONE', #12023, #12670 ) ;
#1955 = ORIENTED_EDGE ( 'NONE', *, *, #1605, .T. ) ;
#1956 = CARTESIAN_POINT ( 'NONE',  ( 34.25000000000000000, 93.41869858279433458, -3.000000000000000888 ) ) ;
#1957 = EDGE_LOOP ( 'NONE', ( #2157, #3202 ) ) ;
#1958 = DIRECTION ( 'NONE',  ( 1.000000000000000000, 0.000000000000000000, 0.000000000000000000 ) ) ;
#1959 = STYLED_ITEM ( 'NONE', ( #8256 ), #8095 ) ;
#1960 = DIRECTION ( 'NONE',  ( 1.000000000000000000, 0.000000000000000000, 0.000000000000000000 ) ) ;
#1961 = ORIENTED_EDGE ( 'NONE', *, *, #5470, .T. ) ;
#1962 = EDGE_CURVE ( 'NONE', #3599, #4788, #1071, .T. ) ;
#1963 = VECTOR ( 'NONE', #8093, 1000.000000000000114 ) ;
#1964 = EDGE_CURVE ( 'NONE', #2737, #10645, #811, .T. ) ;
#1965 = ORIENTED_EDGE ( 'NONE', *, *, #3451, .F. ) ;
#1966 = CARTESIAN_POINT ( 'NONE',  ( 60.00000000000000000, -6.000000000000000000, 15.00000000000000000 ) ) ;
#1967 = ORIENTED_EDGE ( 'NONE', *, *, #5239, .F. ) ;
#1968 = DIRECTION ( 'NONE',  ( 0.000000000000000000, 0.000000000000000000, -1.000000000000000000 ) ) ;
#1969 = AXIS2_PLACEMENT_3D ( 'NONE', #11884, #6908, #10177 ) ;
#1970 = ORIENTED_EDGE ( 'NONE', *, *, #9131, .F. ) ;
#1971 = CARTESIAN_POINT ( 'NONE',  ( 35.00000000000000000, 126.3079067962035822, 3.790625000614517237 ) ) ;
#1972 = EDGE_LOOP ( 'NONE', ( #9502, #4976, #6099, #1965, #9834, #3104, #3537, #1858 ) ) ;
#1973 = DIRECTION ( 'NONE',  ( -0.000000000000000000, 0.5000000000000003331, -0.8660254037844383745 ) ) ;
#1974 = AXIS2_PLACEMENT_3D ( 'NONE', #7887, #5726, #5977 ) ;
#1975 = CARTESIAN_POINT ( 'NONE',  ( 19.27821517812500574, 117.2309300971526937, 3.378125000614517148 ) ) ;
#1976 = VECTOR ( 'NONE', #2128, 1000.000000000000000 ) ;
#1977 = CARTESIAN_POINT ( 'NONE',  ( 48.49999999999995737, 90.00000000000000000, -8.000000000000000000 ) ) ;
#1978 = CARTESIAN_POINT ( 'NONE',  ( 66.19999999999997442, 108.0133283987163253, 4.025000001229034119 ) ) ;
#1979 = EDGE_CURVE ( 'NONE', #8306, #6159, #5913, .T. ) ;
#1980 = DIRECTION ( 'NONE',  ( -0.5000000000000043299, 0.8660254037844362651, 0.000000000000000000 ) ) ;
#1981 = ORIENTED_EDGE ( 'NONE', *, *, #4046, .F. ) ;
#1982 = CARTESIAN_POINT ( 'NONE',  ( 1.040000000000000036, -0.5773502691896255090, 1.000000000000000000 ) ) ;
#1983 = CIRCLE ( 'NONE', #8671, 3.350000000000000089 ) ;
#1984 = CARTESIAN_POINT ( 'NONE',  ( 34.25000000000000000, 93.26496554346289258, 4.800000000000000711 ) ) ;
#1985 = DIRECTION ( 'NONE',  ( -1.000000000000000000, -0.000000000000000000, -0.000000000000000000 ) ) ;
#1986 = VERTEX_POINT ( 'NONE', #12924 ) ;
#1987 = VECTOR ( 'NONE', #986, 1000.000000000000000 ) ;
#1988 = DIRECTION ( 'NONE',  ( -5.624500927088228034E-17, 1.370729058197317775E-18, 1.000000000000000000 ) ) ;
#1989 = VERTEX_POINT ( 'NONE', #3970 ) ;
#1990 = LINE ( 'NONE', #9109, #3375 ) ;
#1991 = CARTESIAN_POINT ( 'NONE',  ( 3.556430356250015024, 90.00000000000000000, 4.409375000614517148 ) ) ;
#1992 = ORIENTED_EDGE ( 'NONE', *, *, #4002, .F. ) ;
#1993 = CARTESIAN_POINT ( 'NONE',  ( 66.44356964374999563, 90.00000000000000000, 3.284375000614517148 ) ) ;
#1994 = AXIS2_PLACEMENT_3D ( 'NONE', #7112, #2938, #9003 ) ;
#1995 = EDGE_CURVE ( 'NONE', #10403, #1497, #9321, .T. ) ;
#1996 = AXIS2_PLACEMENT_3D ( 'NONE', #11776, #12764, #12891 ) ;
#1997 = SHAPE_REPRESENTATION ( 'MAS-185', ( #12202, #1332, #2392, #275, #10731, #5086, #12404, #4887, #10323, #1541, #4472, #1969, #4690, #8857, #6763, #9696, #11145, #7810, #2804, #11780, #5727 ), #10101 ) ;
#1998 = CARTESIAN_POINT ( 'NONE',  ( 28.68194083117254323, 91.52713075379780605, 4.000000000000000000 ) ) ;
#1999 = FACE_OUTER_BOUND ( 'NONE', #11000, .T. ) ;
#2000 = AXIS2_PLACEMENT_3D ( 'NONE', #9846, #3907, #7032 ) ;
#2001 = DIRECTION ( 'NONE',  ( 0.000000000000000000, 0.000000000000000000, -1.000000000000000000 ) ) ;
#2002 = ADVANCED_FACE ( 'NONE', ( #5130 ), #4352, .F. ) ;
#2003 = EDGE_CURVE ( 'NONE', #2627, #1292, #4292, .T. ) ;
#2004 = VECTOR ( 'NONE', #10111, 1000.000000000000000 ) ;
#2005 = CARTESIAN_POINT ( 'NONE',  ( 31.50000000000000000, 90.00000000000000000, 6.000000000000000000 ) ) ;
#2006 = CARTESIAN_POINT ( 'NONE',  ( 3.556430356250028790, 71.84604660189818048, 4.446875000614517681 ) ) ;
#2007 = ORIENTED_EDGE ( 'NONE', *, *, #3459, .F. ) ;
#2008 = DIRECTION ( 'NONE',  ( 0.000000000000000000, 0.000000000000000000, -1.000000000000000000 ) ) ;
#2009 = ORIENTED_EDGE ( 'NONE', *, *, #12275, .T. ) ;
#2010 = DIRECTION ( 'NONE',  ( -0.000000000000000000, -0.000000000000000000, -1.000000000000000000 ) ) ;
#2011 = CIRCLE ( 'NONE', #3694, 31.19999999999999218 ) ;
#2012 = LINE ( 'NONE', #6974, #4777 ) ;
#2013 = DIRECTION ( 'NONE',  ( 0.8090169943749476733, 0.5877852522924726930, 0.000000000000000000 ) ) ;
#2014 = CARTESIAN_POINT ( 'NONE',  ( 66.19999999999998863, 90.00000000000000000, 3.537500001229034297 ) ) ;
#2015 = ORIENTED_EDGE ( 'NONE', *, *, #5500, .T. ) ;
#2016 = DIRECTION ( 'NONE',  ( 0.000000000000000000, 0.000000000000000000, 1.000000000000000000 ) ) ;
#2017 = CONTEXT_DEPENDENT_SHAPE_REPRESENTATION ( #4931, #12131 ) ;
#2018 = CARTESIAN_POINT ( 'NONE',  ( -65.00000000000004263, 38.66025403784436065, -3.000000000000000000 ) ) ;
#2019 = ORIENTED_EDGE ( 'NONE', *, *, #7283, .F. ) ;
#2020 = DIRECTION ( 'NONE',  ( 0.000000000000000000, -0.000000000000000000, 1.000000000000000000 ) ) ;
#2021 = ORIENTED_EDGE ( 'NONE', *, *, #7692, .F. ) ;
#2022 = AXIS2_PLACEMENT_3D ( 'NONE', #4342, #7346, #8463 ) ;
#2023 = DIRECTION ( 'NONE',  ( -0.3262398754384822630, 0.9452870165584014162, 0.000000000000000000 ) ) ;
#2024 = EDGE_LOOP ( 'NONE', ( #3519, #4907, #10756, #11768 ) ) ;
#2025 = EDGE_CURVE ( 'NONE', #6338, #1104, #12661, .T. ) ;
#2026 = DIRECTION ( 'NONE',  ( 5.624500927088228034E-17, -1.370729058197317775E-18, -1.000000000000000000 ) ) ;
#2027 = DIRECTION ( 'NONE',  ( 0.000000000000000000, 0.000000000000000000, 1.000000000000000000 ) ) ;
#2028 = EDGE_LOOP ( 'NONE', ( #2316, #6397, #9153, #3795 ) ) ;
#2029 = ORIENTED_EDGE ( 'NONE', *, *, #3482, .T. ) ;
#2030 = VECTOR ( 'NONE', #7637, 1000.000000000000000 ) ;
#2031 = DIRECTION ( 'NONE',  ( -0.000000000000000000, -0.000000000000000000, -1.000000000000000000 ) ) ;
#2032 = VERTEX_POINT ( 'NONE', #5197 ) ;
#2033 = CARTESIAN_POINT ( 'NONE',  ( 66.19999999999997442, 108.0133283987163253, 4.475000001229034297 ) ) ;
#2034 = ORIENTED_EDGE ( 'NONE', *, *, #10337, .F. ) ;
#2035 = EDGE_CURVE ( 'NONE', #4459, #5941, #9122, .T. ) ;
#2036 = FACE_OUTER_BOUND ( 'NONE', #995, .T. ) ;
#2037 = EDGE_LOOP ( 'NONE', ( #575, #9948, #11098, #3, #1099, #1754 ) ) ;
#2038 = CARTESIAN_POINT ( 'NONE',  ( 19.99999999999998224, 90.00000000000000000, -8.000000000000000000 ) ) ;
#2039 = CARTESIAN_POINT ( 'NONE',  ( 50.72178482187499071, 117.2309300971526937, 4.653125000614517504 ) ) ;
#2040 = ADVANCED_FACE ( 'NONE', ( #11080, #2132, #1135, #10367, #80 ), #4099, .F. ) ;
#2041 = CIRCLE ( 'NONE', #569, 1.599999999999990319 ) ;
#2042 =( LENGTH_UNIT ( ) NAMED_UNIT ( * ) SI_UNIT ( .MILLI., .METRE. ) );
#2043 = DIRECTION ( 'NONE',  ( 0.000000000000000000, 0.000000000000000000, -1.000000000000000000 ) ) ;
#2044 =( LENGTH_UNIT ( ) NAMED_UNIT ( * ) SI_UNIT ( .MILLI., .METRE. ) );
#2045 = DIRECTION ( 'NONE',  ( 0.000000000000000000, 0.000000000000000000, 1.000000000000000000 ) ) ;
#2046 = ORIENTED_EDGE ( 'NONE', *, *, #7362, .F. ) ;
#2047 = CARTESIAN_POINT ( 'NONE',  ( 35.00000000000000711, 53.97334320256736362, 4.212500000000000355 ) ) ;
#2048 = CARTESIAN_POINT ( 'NONE',  ( 62.73303611935715196, 98.48533184915085315, 4.000000000000000000 ) ) ;
#2049 = CARTESIAN_POINT ( 'NONE',  ( 51.56500827743923310, 116.5679260320323323, 3.000000000000000000 ) ) ;
#2050 = CIRCLE ( 'NONE', #4767, 1.500000000000001332 ) ;
#2051 = ORIENTED_EDGE ( 'NONE', *, *, #4067, .T. ) ;
#2052 = CARTESIAN_POINT ( 'NONE',  ( 5.000000000000004441, 0.000000000000000000, -10.00000000000000000 ) ) ;
#2053 = ORIENTED_EDGE ( 'NONE', *, *, #11546, .T. ) ;
#2054 = EDGE_CURVE ( 'NONE', #1154, #3826, #4160, .T. ) ;
#2055 = LINE ( 'NONE', #7149, #8796 ) ;
#2056 = CARTESIAN_POINT ( 'NONE',  ( 64.54728994471078352, 100.7543353520590870, 2.802601390178781404 ) ) ;
#2057 = ORIENTED_EDGE ( 'NONE', *, *, #422, .T. ) ;
#2058 = CARTESIAN_POINT ( 'NONE',  ( 35.00000000000000000, 126.3079067962036106, 4.746875000614517504 ) ) ;
#2059 = FACE_OUTER_BOUND ( 'NONE', #3684, .T. ) ;
#2060 = VECTOR ( 'NONE', #11693, 1000.000000000000000 ) ;
#2062 = AXIS2_PLACEMENT_3D ( 'NONE', #4186, #8173, #7186 ) ;
#2061 = CARTESIAN_POINT ( 'NONE',  ( 0.000000000000000000, 1.154700538379252350, -1.084202172485497162E-16 ) ) ;
#2063 = LINE ( 'NONE', #6770, #3657 ) ;
#2064 = DIRECTION ( 'NONE',  ( 0.000000000000000000, -0.000000000000000000, 1.000000000000000000 ) ) ;
#2065 = CARTESIAN_POINT ( 'NONE',  ( 0.1999999999999965694, -6.446898479113814417, -0.8000000000000000444 ) ) ;
#2066 = EDGE_CURVE ( 'NONE', #7103, #11106, #12136, .T. ) ;
#2067 = VECTOR ( 'NONE', #1199, 1000.000000000000000 ) ;
#2068 = DIRECTION ( 'NONE',  ( -1.000000000000000000, 0.000000000000000000, -0.000000000000000000 ) ) ;
#2069 = FACE_OUTER_BOUND ( 'NONE', #3154, .T. ) ;
#2070 = ORIENTED_EDGE ( 'NONE', *, *, #6607, .T. ) ;
#2071 = LINE ( 'NONE', #2866, #9761 ) ;
#2072 = ORIENTED_EDGE ( 'NONE', *, *, #4557, .F. ) ;
#2073 =( LENGTH_UNIT ( ) NAMED_UNIT ( * ) SI_UNIT ( .MILLI., .METRE. ) );
#2074 = CIRCLE ( 'NONE', #1443, 4.000000000000000000 ) ;
#2075 = EDGE_CURVE ( 'NONE', #3524, #1694, #2330, .T. ) ;
#2076 = AXIS2_PLACEMENT_3D ( 'NONE', #8907, #3819, #6686 ) ;
#2077 = ADVANCED_FACE ( 'NONE', ( #3184 ), #10297, .T. ) ;
#2078 = CARTESIAN_POINT ( 'NONE',  ( 3.800000000000015365, 90.00000000000000000, 3.650000000000000355 ) ) ;
#2079 = DIRECTION ( 'NONE',  ( 0.000000000000000000, 0.000000000000000000, 1.000000000000000000 ) ) ;
#2080 = PLANE ( 'NONE',  #9893 ) ;
#2081 = VERTEX_POINT ( 'NONE', #10100 ) ;
#2082 = CARTESIAN_POINT ( 'NONE',  ( 25.00000000000000355, 2.000000000000000000, -7.349999999999991651 ) ) ;
#2083 = CARTESIAN_POINT ( 'NONE',  ( 19.40000000000002700, 62.98000740192551206, 3.725000000000000089 ) ) ;
#2084 = ORIENTED_EDGE ( 'NONE', *, *, #11517, .F. ) ;
#2085 = AXIS2_PLACEMENT_3D ( 'NONE', #6228, #1187, #128 ) ;
#2086 = EDGE_CURVE ( 'NONE', #977, #10652, #343, .T. ) ;
#2087 = ORIENTED_EDGE ( 'NONE', *, *, #7886, .F. ) ;
#2088 = APPLICATION_CONTEXT ( 'automotive_design' ) ;
#2089 = CARTESIAN_POINT ( 'NONE',  ( -31.49999999999998579, 46.45448267190452896, 1.000000000000000000 ) ) ;
#2090 = ORIENTED_EDGE ( 'NONE', *, *, #9698, .T. ) ;
#2091 = DIRECTION ( 'NONE',  ( 0.4719909656437444867, -0.8816033849473842166, 0.000000000000000000 ) ) ;
#2092 = CARTESIAN_POINT ( 'NONE',  ( 64.54728994471078352, 100.7543353520590870, 2.802601390178781404 ) ) ;
#2093 = ORIENTED_EDGE ( 'NONE', *, *, #7600, .T. ) ;
#2094 = EDGE_CURVE ( 'NONE', #919, #1862, #8889, .T. ) ;
#2095 = AXIS2_PLACEMENT_3D ( 'NONE', #2749, #4771, #1887 ) ;
#2096 = VERTEX_POINT ( 'NONE', #3116 ) ;
#2097 = DIRECTION ( 'NONE',  ( 0.000000000000000000, 0.000000000000000000, 1.000000000000000000 ) ) ;
#2098 = ORIENTED_EDGE ( 'NONE', *, *, #7758, .F. ) ;
#2099 = CARTESIAN_POINT ( 'NONE',  ( -6.666666666666660745, 6.415593491261681436, -1.734723475976807094E-15 ) ) ;
#2100 = CARTESIAN_POINT ( 'NONE',  ( 3.556430356250028790, 71.84604660189818048, 4.390625000614517326 ) ) ;
#2101 = VERTEX_POINT ( 'NONE', #7161 ) ;
#2102 = LINE ( 'NONE', #12040, #7594 ) ;
#2103 = ORIENTED_EDGE ( 'NONE', *, *, #10688, .T. ) ;
#2104 = VECTOR ( 'NONE', #11623, 1000.000000000000000 ) ;
#2105 = CARTESIAN_POINT ( 'NONE',  ( 1.040000000000000036, -0.5773502691896253980, -1.000000000000000000 ) ) ;
#2106 = AXIS2_PLACEMENT_3D ( 'NONE', #1133, #12199, #12265 ) ;
#2107 = CARTESIAN_POINT ( 'NONE',  ( 3.556430356250028790, 71.84604660189818048, 3.040625000614517681 ) ) ;
#2108 = CARTESIAN_POINT ( 'NONE',  ( 35.00000000000000000, 90.00000000000000000, 4.800000000000000711 ) ) ;
#2109 = CARTESIAN_POINT ( 'NONE',  ( 3.800000000000025135, 71.98667160128366049, 3.800000001229034030 ) ) ;
#2110 = DIRECTION ( 'NONE',  ( -0.8665440819333538602, -0.4991005450470686888, -4.805464830191153728E-17 ) ) ;
#2111 = ORIENTED_EDGE ( 'NONE', *, *, #9460, .T. ) ;
#2112 = VECTOR ( 'NONE', #11928, 1000.000000000000000 ) ;
#2113 = CARTESIAN_POINT ( 'NONE',  ( 66.44356964374998142, 108.1539533981018053, 4.671875000614516438 ) ) ;
#2114 = EDGE_CURVE ( 'NONE', #1140, #5477, #2200, .T. ) ;
#2115 = CARTESIAN_POINT ( 'NONE',  ( 25.00000000000000355, 0.000000000000000000, -5.750000000000000000 ) ) ;
#2116 = CARTESIAN_POINT ( 'NONE',  ( 50.47081135474928715, 117.2246076195576734, 3.000000000000001332 ) ) ;
#2117 = ORIENTED_EDGE ( 'NONE', *, *, #10147, .T. ) ;
#2118 = PLANE ( 'NONE',  #3215 ) ;
#2119 = ORIENTED_EDGE ( 'NONE', *, *, #214, .T. ) ;
#2120 = LINE ( 'NONE', #9835, #10672 ) ;
#2121 = UNCERTAINTY_MEASURE_WITH_UNIT (LENGTH_MEASURE( 1.000000000000000082E-05 ), #3271, 'distance_accuracy_value', 'NONE');
#2122 = CARTESIAN_POINT ( 'NONE',  ( 50.72178482187501203, 62.76906990284730625, 3.603125000614517681 ) ) ;
#2123 = VERTEX_POINT ( 'NONE', #4227 ) ;
#2124 = CARTESIAN_POINT ( 'NONE',  ( 19.27821517812500574, 117.2309300971526937, 3.884375000614516793 ) ) ;
#2125 = DIRECTION ( 'NONE',  ( 1.000000000000000000, 0.000000000000000000, 5.337610695313252124E-17 ) ) ;
#2126 = CARTESIAN_POINT ( 'NONE',  ( 40.00000000000000000, 2.000000000000000000, -1.499999999999999556 ) ) ;
#2127 = EDGE_CURVE ( 'NONE', #718, #309, #8213, .T. ) ;
#2128 = DIRECTION ( 'NONE',  ( 0.000000000000000000, 0.000000000000000000, 1.000000000000000000 ) ) ;
#2129 = EDGE_CURVE ( 'NONE', #3989, #3015, #7231, .T. ) ;
#2130 = CARTESIAN_POINT ( 'NONE',  ( 0.000000000000000000, 0.5773502691896262862, 1.000000000000000000 ) ) ;
#2131 = AXIS2_PLACEMENT_3D ( 'NONE', #7843, #10790, #2023 ) ;
#2132 = FACE_BOUND ( 'NONE', #11150, .T. ) ;
#2133 = FACE_OUTER_BOUND ( 'NONE', #10319, .T. ) ;
#2134 = CARTESIAN_POINT ( 'NONE',  ( -60.00000000000000000, 0.000000000000000000, -10.00000000000000355 ) ) ;
#2135 = EDGE_LOOP ( 'NONE', ( #6787, #2219, #4205, #4367, #1961, #1404 ) ) ;
#2136 = FACE_BOUND ( 'NONE', #12116, .T. ) ;
#2137 = ORIENTED_EDGE ( 'NONE', *, *, #5023, .F. ) ;
#2138 =( LENGTH_UNIT ( ) NAMED_UNIT ( * ) SI_UNIT ( .MILLI., .METRE. ) );
#2139 = ADVANCED_FACE ( 'NONE', ( #10235 ), #6382, .F. ) ;
#2140 = LINE ( 'NONE', #7241, #1208 ) ;
#2141 = CARTESIAN_POINT ( 'NONE',  ( 66.19999999999998863, 90.00000000000000000, 3.987500001229034030 ) ) ;
#2142 = DIRECTION ( 'NONE',  ( 0.000000000000000000, 0.000000000000000000, 1.000000000000000000 ) ) ;
#2143 = EDGE_CURVE ( 'NONE', #10857, #8362, #12026, .T. ) ;
#2144 = ORIENTED_EDGE ( 'NONE', *, *, #653, .T. ) ;
#2145 = CARTESIAN_POINT ( 'NONE',  ( 35.00000000000000000, 90.00000000000000000, -3.799999999999999378 ) ) ;
#2146 = CARTESIAN_POINT ( 'NONE',  ( 3.800000000000004707, 90.00000000000000000, 6.000000000000000000 ) ) ;
#2147 = ORIENTED_EDGE ( 'NONE', *, *, #12555, .F. ) ;
#2148 = AXIS2_PLACEMENT_3D ( 'NONE', #11822, #5987, #2990 ) ;
#2149 =( BOUNDED_SURFACE ( )  B_SPLINE_SURFACE ( 1, 2, ( 
 ( #801, #2721, #6694, #9836, #11929, #7808, #2974, #11865, #10752, #7878, #1860, #12785, #1991, #9897, #1796, #10939, #5847, #8666, #12914, #8854, #5969, #864, #3828, #12662, #6955, #4934, #741, #4867, #5718, #672, #12850, #2783, #3898, #3704, #6891, #7685, #5782, #10879, #11804, #11670, #7746, #6823, #11733, #10690, #1924, #929, #1731, #9705, #4741, #8728, #12723, #3764, #6761, #9772, #4806 ),
 ( #6098, #997, #264, #2, #3106, #3038, #4023, #7219, #1059, #7022, #5186, #2259, #1125, #1261, #3306, #11003, #8008, #1194, #4995, #7088, #6235, #10159, #12189, #198, #2322, #11070, #9175, #4216, #11990, #10225, #9044, #8203, #2122, #3239, #10089, #8979, #5119, #11133, #9110, #3173, #6035, #8073, #11206, #10029, #4086, #6166, #5253, #9966, #12060, #9241, #4281, #134, #8269, #12258, #2056 ) ),
 .UNSPECIFIED., .F., .F., .F. ) 
 B_SPLINE_SURFACE_WITH_KNOTS ( ( 2, 2 ),
 ( 3, 2, 2, 2, 2, 2, 2, 2, 2, 2, 2, 2, 2, 2, 2, 2, 2, 2, 2, 2, 2, 2, 2, 2, 2, 2, 2, 3 ),
 ( 0.000000000000000000, 1.000000000000000000 ),
 ( 0.000000000000000000, 0.03333333333333333287, 0.06666666666666666574, 0.1000000000000000056, 0.1333333333333333315, 0.1666666666666666574, 0.2000000000000000111, 0.2333333333333333370, 0.2666666666666666630, 0.2999999999999999889, 0.3333333333333333148, 0.3666666666666666408, 0.4000000000000000222, 0.4333333333333333481, 0.4666666666666666741, 0.5000000000000000000, 0.5333333333333333259, 0.5666666666666666519, 0.5999999999999999778, 0.6333333333333333037, 0.6666666666666666297, 0.6999999999999999556, 0.7333333333333332815, 0.7666666666666667185, 0.8000000000000000444, 0.8333333333333333703, 0.8666666666666666963, 0.8887752010635167066 ),
 .UNSPECIFIED. ) 
 GEOMETRIC_REPRESENTATION_ITEM ( )  RATIONAL_B_SPLINE_SURFACE ( (
 ( 1.000000000000000000, 0.8660254037844387076, 1.000000000000000000, 0.8660254037844387076, 1.000000000000000000, 0.8660254037844387076, 1.000000000000000000, 0.8660254037844387076, 1.000000000000000000, 0.8660254037844387076, 1.000000000000000000, 0.8660254037844387076, 1.000000000000000000, 0.8660254037844387076, 1.000000000000000000, 0.8660254037844387076, 1.000000000000000000, 0.8660254037844387076, 1.000000000000000000, 0.8660254037844387076, 1.000000000000000000, 0.8660254037844387076, 1.000000000000000000, 0.8660254037844387076, 1.000000000000000000, 0.8660254037844387076, 1.000000000000000000, 0.8660254037844387076, 1.000000000000000000, 0.8660254037844387076, 1.000000000000000000, 0.8660254037844387076, 1.000000000000000000, 0.8660254037844387076, 1.000000000000000000, 0.8660254037844387076, 1.000000000000000000, 0.8660254037844387076, 1.000000000000000000, 0.8660254037844387076, 1.000000000000000000, 0.8660254037844387076, 1.000000000000000000, 0.8660254037844387076, 1.000000000000000000, 0.8660254037844387076, 1.000000000000000000, 0.8660254037844387076, 1.000000000000000000, 0.8660254037844387076, 1.000000000000000000, 0.8660254037844387076, 1.000000000000000000, 0.9111405409379251807, 0.9401542263054123438),
 ( 1.000000000000000000, 0.8660254037844387076, 1.000000000000000000, 0.8660254037844387076, 1.000000000000000000, 0.8660254037844387076, 1.000000000000000000, 0.8660254037844387076, 1.000000000000000000, 0.8660254037844387076, 1.000000000000000000, 0.8660254037844387076, 1.000000000000000000, 0.8660254037844387076, 1.000000000000000000, 0.8660254037844387076, 1.000000000000000000, 0.8660254037844387076, 1.000000000000000000, 0.8660254037844387076, 1.000000000000000000, 0.8660254037844387076, 1.000000000000000000, 0.8660254037844387076, 1.000000000000000000, 0.8660254037844387076, 1.000000000000000000, 0.8660254037844387076, 1.000000000000000000, 0.8660254037844387076, 1.000000000000000000, 0.8660254037844387076, 1.000000000000000000, 0.8660254037844387076, 1.000000000000000000, 0.8660254037844387076, 1.000000000000000000, 0.8660254037844387076, 1.000000000000000000, 0.8660254037844387076, 1.000000000000000000, 0.8660254037844387076, 1.000000000000000000, 0.8660254037844387076, 1.000000000000000000, 0.8660254037844387076, 1.000000000000000000, 0.8660254037844387076, 1.000000000000000000, 0.8660254037844387076, 1.000000000000000000, 0.8660254037844387076, 1.000000000000000000, 0.9111405409379251807, 0.9401542263054123438) ) ) 
 REPRESENTATION_ITEM ( '' )  SURFACE ( )  );
#2150 = PRESENTATION_STYLE_ASSIGNMENT (( #3001 ) ) ;
#2151 = PRESENTATION_STYLE_ASSIGNMENT (( #11097 ) ) ;
#2152 = EDGE_LOOP ( 'NONE', ( #6828, #7770, #5880, #2183, #806, #9980 ) ) ;
#2153 = CARTESIAN_POINT ( 'NONE',  ( 20.00000000000000355, 2.000000000000001776, 1.500000000000000444 ) ) ;
#2154 = ORIENTED_EDGE ( 'NONE', *, *, #12163, .T. ) ;
#2155 = CARTESIAN_POINT ( 'NONE',  ( 1.040000000000000036, -1.154700538379251684, 0.000000000000000000 ) ) ;
#2156 = ORIENTED_EDGE ( 'NONE', *, *, #5971, .T. ) ;
#2157 = ORIENTED_EDGE ( 'NONE', *, *, #5870, .F. ) ;
#2158 = CARTESIAN_POINT ( 'NONE',  ( 13.22666678878058200, 110.6378768499380527, -1.000000000000000000 ) ) ;
#2159 = ORIENTED_EDGE ( 'NONE', *, *, #7690, .F. ) ;
#2160 = CIRCLE ( 'NONE', #6333, 1.425000000000000044 ) ;
#2161 = APPLICATION_PROTOCOL_DEFINITION ( 'draft international standard', 'automotive_design', 1998, #8533 ) ;
#2162 = CARTESIAN_POINT ( 'NONE',  ( 19.27821517812503060, 62.76906990284727783, 3.078125000614517326 ) ) ;
#2163 = ORIENTED_EDGE ( 'NONE', *, *, #10289, .T. ) ;
#2164 = CARTESIAN_POINT ( 'NONE',  ( 3.800000000000015365, 90.00000000000000000, 3.312500001229034652 ) ) ;
#2165 = LINE ( 'NONE', #9155, #2496 ) ;
#2166 = EDGE_CURVE ( 'NONE', #9809, #169, #7487, .T. ) ;
#2167 = ORIENTED_EDGE ( 'NONE', *, *, #4353, .T. ) ;
#2168 = ADVANCED_FACE ( 'NONE', ( #606 ), #12528, .T. ) ;
#2169 = COLOUR_RGB ( '',1.000000000000000000, 0.9490196078431372140, 0.9098039215686274384 ) ;
#2170 = ADVANCED_BREP_SHAPE_REPRESENTATION ( '', ( #11791, #5704 ), #1096 ) ;
#2171 = CARTESIAN_POINT ( 'NONE',  ( 34.25000000000000000, 93.41869858279433458, 22.38477631085024555 ) ) ;
#2172 = CARTESIAN_POINT ( 'NONE',  ( 66.44356964374999563, 90.00000000000000000, 4.578125000614516438 ) ) ;
#2173 =( NAMED_UNIT ( * ) SI_UNIT ( $, .STERADIAN. ) SOLID_ANGLE_UNIT ( ) );
#2174 = DIRECTION ( 'NONE',  ( 0.000000000000000000, 0.000000000000000000, -1.000000000000000000 ) ) ;
#2175 = AXIS2_PLACEMENT_3D ( 'NONE', #1017, #5014, #6849 ) ;
#2176 = CARTESIAN_POINT ( 'NONE',  ( 21.49999999999998579, 86.00000000000000000, -10.00000000000000000 ) ) ;
#2177 = VERTEX_POINT ( 'NONE', #3572 ) ;
#2178 = PRODUCT_DEFINITION_FORMATION_WITH_SPECIFIED_SOURCE ( 'ANY', '', #282, .NOT_KNOWN. ) ;
#2179 = CARTESIAN_POINT ( 'NONE',  ( 3.800000000000025135, 71.98667160128366049, 4.137500000000001066 ) ) ;
#2180 = ORIENTED_EDGE ( 'NONE', *, *, #1766, .F. ) ;
#2181 = CARTESIAN_POINT ( 'NONE',  ( -23.49999999999999289, 79.07477288111861924, 1.000000000000000000 ) ) ;
#2182 = DIRECTION ( 'NONE',  ( 1.000000000000000000, 0.000000000000000000, 0.000000000000000000 ) ) ;
#2183 = ORIENTED_EDGE ( 'NONE', *, *, #9832, .F. ) ;
#2184 = AXIS2_PLACEMENT_3D ( 'NONE', #4876, #10697, #2791 ) ;
#2185 = DIRECTION ( 'NONE',  ( 0.4719909656437442647, -0.8816033849473842166, 2.775557561595757269E-17 ) ) ;
#2186 = ORIENTED_EDGE ( 'NONE', *, *, #7665, .F. ) ;
#2187 = AXIS2_PLACEMENT_3D ( 'NONE', #1931, #9118, #1132 ) ;
#2188 = DIRECTION ( 'NONE',  ( 0.000000000000000000, 0.000000000000000000, 1.000000000000000000 ) ) ;
#2189 = CARTESIAN_POINT ( 'NONE',  ( 62.42406877824604550, 99.43633191144624561, -1.000000000000000222 ) ) ;
#2190 = VERTEX_POINT ( 'NONE', #10493 ) ;
#2191 = CARTESIAN_POINT ( 'NONE',  ( 50.72178482187501203, 62.76906990284730625, 4.109375000614517326 ) ) ;
#2192 = PLANE ( 'NONE',  #10824 ) ;
#2193 = ADVANCED_FACE ( 'NONE', ( #12593 ), #3441, .T. ) ;
#2194 = CARTESIAN_POINT ( 'NONE',  ( 63.99885733073619321, 89.74256357754357794, 4.000000000000000000 ) ) ;
#2195 = CIRCLE ( 'NONE', #3245, 1.500000000000000222 ) ;
#2196 = TOROIDAL_SURFACE ( 'NONE', #9294, 1.599999999999999645, 0.1000000000000000056 ) ;
#2197 = SURFACE_STYLE_FILL_AREA ( #936 ) ;
#2198 = DIRECTION ( 'NONE',  ( 0.000000000000000000, 0.000000000000000000, 1.000000000000000000 ) ) ;
#2199 = DIRECTION ( 'NONE',  ( -0.4999999999999985012, 0.8660254037844394848, 0.000000000000000000 ) ) ;
#2200 = LINE ( 'NONE', #6178, #1795 ) ;
#2201 = ADVANCED_FACE ( 'NONE', ( #1465 ), #670, .T. ) ;
#2202 = DIRECTION ( 'NONE',  ( 0.000000000000000000, 0.000000000000000000, 1.000000000000000000 ) ) ;
#2203 = AXIS2_PLACEMENT_3D ( 'NONE', #9334, #8226, #356 ) ;
#2204 = CARTESIAN_POINT ( 'NONE',  ( 19.27821517812503060, 62.76906990284727783, 3.134375000614517237 ) ) ;
#2205 = ORIENTED_EDGE ( 'NONE', *, *, #7737, .T. ) ;
#2206 = AXIS2_PLACEMENT_3D ( 'NONE', #5682, #7902, #11889 ) ;
#2207 = CARTESIAN_POINT ( 'NONE',  ( 48.49999999999995737, 90.00000000000000000, -10.00000000000000000 ) ) ;
#2208 = ORIENTED_EDGE ( 'NONE', *, *, #7500, .T. ) ;
#2209 = EDGE_CURVE ( 'NONE', #1825, #4500, #9447, .T. ) ;
#2210 = DIRECTION ( 'NONE',  ( -1.000000000000000000, 0.000000000000000000, 0.000000000000000000 ) ) ;
#2211 = CARTESIAN_POINT ( 'NONE',  ( 50.59999999999999432, 117.0199925980744666, 4.062500001229034652 ) ) ;
#2212 = VECTOR ( 'NONE', #11144, 1000.000000000000114 ) ;
#2213 = PRODUCT_DEFINITION_SHAPE ( 'NONE', 'NONE',  #12971 ) ;
#2214 = PLANE ( 'NONE',  #6768 ) ;
#2215 = VECTOR ( 'NONE', #9482, 1000.000000000000000 ) ;
#2216 = ORIENTED_EDGE ( 'NONE', *, *, #3696, .T. ) ;
#2217 = PLANE ( 'NONE',  #4496 ) ;
#2218 = CARTESIAN_POINT ( 'NONE',  ( 30.78620769635677235, 85.05086326499690585, 22.38477631085024555 ) ) ;
#2219 = ORIENTED_EDGE ( 'NONE', *, *, #10889, .F. ) ;
#2220 = FILL_AREA_STYLE ('',( #12221 ) ) ;
#2221 = CARTESIAN_POINT ( 'NONE',  ( 63.68224097532933570, 98.79369391286385849, -3.000000000000000000 ) ) ;
#2222 = ORIENTED_EDGE ( 'NONE', *, *, #596, .F. ) ;
#2223 = EDGE_CURVE ( 'NONE', #3511, #12839, #2429, .T. ) ;
#2224 = PLANE ( 'NONE',  #11311 ) ;
#2226 = ORIENTED_EDGE ( 'NONE', *, *, #3194, .F. ) ;
#2225 = CIRCLE ( 'NONE', #4933, 3.500000000000003109 ) ;
#2227 = AXIS2_PLACEMENT_3D ( 'NONE', #12883, #8886, #5813 ) ;
#2228 = DIRECTION ( 'NONE',  ( -1.000000000000000000, 0.000000000000000000, -0.000000000000000000 ) ) ;
#2229 = CARTESIAN_POINT ( 'NONE',  ( -61.00000000000000711, 31.73205080756887142, 3.000000000000000000 ) ) ;
#2230 = ORIENTED_EDGE ( 'NONE', *, *, #7511, .F. ) ;
#2231 = ORIENTED_EDGE ( 'NONE', *, *, #6103, .T. ) ;
#2232 = CARTESIAN_POINT ( 'NONE',  ( 33.50000000000000711, 67.79999999999999716, 8.000000000000000000 ) ) ;
#2233 = ORIENTED_EDGE ( 'NONE', *, *, #8141, .T. ) ;
#2234 = DIRECTION ( 'NONE',  ( -1.000000000000000000, 0.000000000000000000, 0.000000000000000000 ) ) ;
#2235 = CARTESIAN_POINT ( 'NONE',  ( 19.27821517812503060, 62.76906990284727783, 3.978125000614516793 ) ) ;
#2236 = VECTOR ( 'NONE', #595, 1000.000000000000000 ) ;
#2237 = ORIENTED_EDGE ( 'NONE', *, *, #12195, .F. ) ;
#2238 = CARTESIAN_POINT ( 'NONE',  ( 0.000000000000000000, 0.000000000000000000, 0.000000000000000000 ) ) ;
#2239 = CARTESIAN_POINT ( 'NONE',  ( -61.13397459621560159, 31.96410161513775350, 0.000000000000000000 ) ) ;
#2240 = VERTEX_POINT ( 'NONE', #10625 ) ;
#2241 = EDGE_CURVE ( 'NONE', #12941, #11688, #2718, .T. ) ;
#2242 = DIRECTION ( 'NONE',  ( 5.337610695313252124E-17, 0.000000000000000000, -1.000000000000000000 ) ) ;
#2243 = CARTESIAN_POINT ( 'NONE',  ( 66.44356964375000985, 71.84604660189820891, 3.640625000614517326 ) ) ;
#2244 = DIRECTION ( 'NONE',  ( 0.000000000000000000, 1.000000000000000000, 0.000000000000000000 ) ) ;
#2245 = DIRECTION ( 'NONE',  ( 1.914177628664063178E-15, -1.000000000000000000, 0.000000000000000000 ) ) ;
#2246 = AXIS2_PLACEMENT_3D ( 'NONE', #5889, #9882, #787 ) ;
#2247 = CARTESIAN_POINT ( 'NONE',  ( 1.269999999999999796, 0.000000000000000000, 2.849999999999999201 ) ) ;
#2248 = EDGE_CURVE ( 'NONE', #7938, #6066, #5129, .T. ) ;
#2250 = EDGE_CURVE ( 'NONE', #2096, #9602, #2849, .T. ) ;
#2249 = ORIENTED_EDGE ( 'NONE', *, *, #57, .T. ) ;
#2251 = CARTESIAN_POINT ( 'NONE',  ( 19.40000000000002700, 62.98000740192551206, 3.275000000000000355 ) ) ;
#2252 = CARTESIAN_POINT ( 'NONE',  ( -4.763019983628629994, -4.349268977144818749, -0.8000000000000000444 ) ) ;
#2253 = EDGE_LOOP ( 'NONE', ( #9736, #12024, #1577, #9723 ) ) ;
#2254 = CARTESIAN_POINT ( 'NONE',  ( 1.649999999999999023, 1.959434878635763258E-16, -1.599999999999998757 ) ) ;
#2255 = ORIENTED_EDGE ( 'NONE', *, *, #9162, .T. ) ;
#2256 = VECTOR ( 'NONE', #11478, 1000.000000000000114 ) ;
#2257 = LINE ( 'NONE', #3238, #4625 ) ;
#2258 = EDGE_CURVE ( 'NONE', #4025, #3338, #5451, .T. ) ;
#2259 = CARTESIAN_POINT ( 'NONE',  ( 3.556430356250028790, 71.84604660189818048, 4.390625000614517326 ) ) ;
#2260 = CARTESIAN_POINT ( 'NONE',  ( 19.27821517812500574, 117.2309300971526937, 4.334375000614516971 ) ) ;
#2261 = DIRECTION ( 'NONE',  ( 0.000000000000000000, 0.000000000000000000, 1.000000000000000000 ) ) ;
#2262 = PLANE ( 'NONE',  #1227 ) ;
#2263 = CIRCLE ( 'NONE', #8318, 3.351416843938785028 ) ;
#2264 = CARTESIAN_POINT ( 'NONE',  ( 1.649999999999999911, 1.959434878635764737E-16, -1.599999999999999645 ) ) ;
#2265 = CARTESIAN_POINT ( 'NONE',  ( 52.49999999999996447, 94.00000000000000000, -10.00000000000000000 ) ) ;
#2266 = DIRECTION ( 'NONE',  ( -0.000000000000000000, 1.000000000000000000, -0.000000000000000000 ) ) ;
#2267 = APPLICATION_CONTEXT ( 'automotive_design' ) ;
#2268 = CARTESIAN_POINT ( 'NONE',  ( 45.00000000000000000, 2.000000000000001332, -5.750000000000000000 ) ) ;
#2269 = EDGE_CURVE ( 'NONE', #12412, #8709, #8408, .T. ) ;
#2270 = CARTESIAN_POINT ( 'NONE',  ( 3.800000000000015365, 90.00000000000000000, 5.000000000000000000 ) ) ;
#2271 = CARTESIAN_POINT ( 'NONE',  ( 13.53859087060910404, 112.9805567844265397, 2.999999999999999112 ) ) ;
#2272 = ORIENTED_EDGE ( 'NONE', *, *, #3616, .F. ) ;
#2273 = VECTOR ( 'NONE', #9361, 1000.000000000000000 ) ;
#2274 = CARTESIAN_POINT ( 'NONE',  ( 52.45028081366923089, 66.83239978927284142, 4.000000000000000000 ) ) ;
#2275 = ORIENTED_EDGE ( 'NONE', *, *, #6757, .T. ) ;
#2276 =( NAMED_UNIT ( * ) PLANE_ANGLE_UNIT ( ) SI_UNIT ( $, .RADIAN. ) );
#2277 = DIRECTION ( 'NONE',  ( -1.000000000000000000, 0.000000000000000000, 0.000000000000000000 ) ) ;
#2278 = DIRECTION ( 'NONE',  ( 0.000000000000000000, 0.000000000000000000, 1.000000000000000000 ) ) ;
#2279 = CARTESIAN_POINT ( 'NONE',  ( 52.45028081366923089, 66.83239978927284142, 4.000000000000000000 ) ) ;
#2280 = VECTOR ( 'NONE', #12698, 1000.000000000000000 ) ;
#2281 = VERTEX_POINT ( 'NONE', #11538 ) ;
#2282 = LINE ( 'NONE', #291, #512 ) ;
#2283 = EDGE_CURVE ( 'NONE', #11574, #998, #4613, .T. ) ;
#2284 = PLANE ( 'NONE',  #12748 ) ;
#2285 = ORIENTED_EDGE ( 'NONE', *, *, #11434, .T. ) ;
#2286 = DIRECTION ( 'NONE',  ( 1.000000000000000000, 0.000000000000000000, 0.000000000000000000 ) ) ;
#2287 = DIRECTION ( 'NONE',  ( -0.000000000000000000, -0.000000000000000000, -1.000000000000000000 ) ) ;
#2288 = ORIENTED_EDGE ( 'NONE', *, *, #1004, .T. ) ;
#2289 = ORIENTED_EDGE ( 'NONE', *, *, #1637, .T. ) ;
#2290 = VECTOR ( 'NONE', #5580, 1000.000000000000000 ) ;
#2291 = DIRECTION ( 'NONE',  ( 5.337610695313252124E-17, 0.000000000000000000, -1.000000000000000000 ) ) ;
#2292 = PLANE ( 'NONE',  #369 ) ;
#2293 = ORIENTED_EDGE ( 'NONE', *, *, #11013, .F. ) ;
#2294 = ADVANCED_FACE ( 'NONE', ( #9642 ), #7422, .F. ) ;
#2295 = ORIENTED_EDGE ( 'NONE', *, *, #987, .F. ) ;
#2297 = CYLINDRICAL_SURFACE ( 'NONE', #2832, 1.500000000000001332 ) ;
#2296 = VECTOR ( 'NONE', #8196, 1000.000000000000000 ) ;
#2298 = ORIENTED_EDGE ( 'NONE', *, *, #11289, .F. ) ;
#2299 = EDGE_CURVE ( 'NONE', #4333, #3861, #12859, .T. ) ;
#2300 = CARTESIAN_POINT ( 'NONE',  ( 21.49999999999998579, 90.00000000000000000, -11.65000000000000036 ) ) ;
#2301 = CARTESIAN_POINT ( 'NONE',  ( 19.27821517812500574, 117.2309300971526937, 4.728125000614516793 ) ) ;
#2302 = AXIS2_PLACEMENT_3D ( 'NONE', #9764, #8659, #7932 ) ;
#2303 = EDGE_LOOP ( 'NONE', ( #10656, #8806, #2505, #6000, #130 ) ) ;
#2304 = DIRECTION ( 'NONE',  ( -1.000000000000000000, -5.551115123125781124E-15, 0.000000000000000000 ) ) ;
#2305 = ORIENTED_EDGE ( 'NONE', *, *, #12144, .T. ) ;
#2306 = DIRECTION ( 'NONE',  ( 0.000000000000000000, 0.000000000000000000, 1.000000000000000000 ) ) ;
#2307 = LINE ( 'NONE', #8254, #11740 ) ;
#2308 = VECTOR ( 'NONE', #625, 1000.000000000000114 ) ;
#2309 = CARTESIAN_POINT ( 'NONE',  ( 3.800000000000015365, 108.0133283987163111, 3.275000001229034119 ) ) ;
#2310 = DIRECTION ( 'NONE',  ( 1.000000000000000000, 0.000000000000000000, -0.000000000000000000 ) ) ;
#2311 = EDGE_CURVE ( 'NONE', #9930, #5561, #6433, .T. ) ;
#2312 = EDGE_LOOP ( 'NONE', ( #11265, #1812, #3367, #4714 ) ) ;
#2313 = CARTESIAN_POINT ( 'NONE',  ( 3.800000000000015365, 90.00000000000000000, 4.100000000000000533 ) ) ;
#2314 = VERTEX_POINT ( 'NONE', #4479 ) ;
#2315 = LINE ( 'NONE', #6351, #2296 ) ;
#2316 = ORIENTED_EDGE ( 'NONE', *, *, #12882, .F. ) ;
#2317 = VECTOR ( 'NONE', #10830, 999.9999999999998863 ) ;
#2318 = ADVANCED_FACE ( 'NONE', ( #8473 ), #12461, .T. ) ;
#2319 = LINE ( 'NONE', #6030, #470 ) ;
#2320 = ORIENTED_EDGE ( 'NONE', *, *, #7949, .F. ) ;
#2321 = LINE ( 'NONE', #5374, #12344 ) ;
#2322 = CARTESIAN_POINT ( 'NONE',  ( 3.556430356250015024, 90.00000000000000000, 3.903125000614517504 ) ) ;
#2323 = ADVANCED_FACE ( 'NONE', ( #7019 ), #4804, .T. ) ;
#2324 = CARTESIAN_POINT ( 'NONE',  ( 50.72178482187501203, 62.76906990284730625, 4.109375000614517326 ) ) ;
#2325 = CARTESIAN_POINT ( 'NONE',  ( 40.00000000000000000, 0.000000000000000000, 10.00000000000000000 ) ) ;
#2326 = CARTESIAN_POINT ( 'NONE',  ( 25.00000000000000355, 0.000000000000000000, 7.250000000000000888 ) ) ;
#2327 = VECTOR ( 'NONE', #197, 1000.000000000000000 ) ;
#2328 = DIRECTION ( 'NONE',  ( -1.000000000000000000, 0.000000000000000000, 0.000000000000000000 ) ) ;
#2329 = CARTESIAN_POINT ( 'NONE',  ( 45.00000000000000000, 2.000000000000000000, -5.750000000000000000 ) ) ;
#2330 = LINE ( 'NONE', #6108, #7434 ) ;
#2331 = VECTOR ( 'NONE', #10659, 1000.000000000000000 ) ;
#2332 = DIRECTION ( 'NONE',  ( 1.000000000000000000, -0.000000000000000000, -0.000000000000000000 ) ) ;
#2333 = CARTESIAN_POINT ( 'NONE',  ( 35.00000000000000711, 53.69209320379639649, 3.171875000614517326 ) ) ;
#2335 = EDGE_CURVE ( 'NONE', #4130, #7314, #2225, .T. ) ;
#2334 = VERTEX_POINT ( 'NONE', #3956 ) ;
#2336 = EDGE_CURVE ( 'NONE', #7731, #6997, #11965, .T. ) ;
#2337 = CARTESIAN_POINT ( 'NONE',  ( 1.649999999999999911, 0.000000000000000000, 2.849999999999999201 ) ) ;
#2338 = ORIENTED_EDGE ( 'NONE', *, *, #1198, .T. ) ;
#2339 = CARTESIAN_POINT ( 'NONE',  ( 23.09999999999997300, 90.00000000000000000, -10.00000000000000000 ) ) ;
#2340 = LINE ( 'NONE', #4364, #2004 ) ;
#2341 = DIRECTION ( 'NONE',  ( -1.000000000000000000, 0.000000000000000000, 0.000000000000000000 ) ) ;
#2342 = ORIENTED_EDGE ( 'NONE', *, *, #3931, .F. ) ;
#2343 = DIRECTION ( 'NONE',  ( 0.000000000000000000, -1.000000000000000000, 0.000000000000000000 ) ) ;
#2344 = FACE_OUTER_BOUND ( 'NONE', #10064, .T. ) ;
#2345 = ORIENTED_EDGE ( 'NONE', *, *, #2733, .F. ) ;
#2346 = CARTESIAN_POINT ( 'NONE',  ( 35.00000000000000000, 90.00000000000000000, -3.799999999999999822 ) ) ;
#2347 = VERTEX_POINT ( 'NONE', #8789 ) ;
#2348 = AXIS2_PLACEMENT_3D ( 'NONE', #6745, #12651, #12585 ) ;
#2349 = PRODUCT_DEFINITION ( 'UNKNOWN', '', #6557, #170 ) ;
#2350 = ORIENTED_EDGE ( 'NONE', *, *, #3130, .T. ) ;
#2351 = DIRECTION ( 'NONE',  ( -1.000000000000000000, 0.000000000000000000, -0.000000000000000000 ) ) ;
#2352 = DIRECTION ( 'NONE',  ( -5.624500927088228034E-17, 1.370729058197317775E-18, 1.000000000000000000 ) ) ;
#2353 = ADVANCED_FACE ( 'NONE', ( #3894 ), #320, .F. ) ;
#2354 = ORIENTED_EDGE ( 'NONE', *, *, #2815, .T. ) ;
#2355 = EDGE_LOOP ( 'NONE', ( #6387, #1563, #6766, #2685 ) ) ;
#2356 = COLOUR_RGB ( '',0.8941176470588234615, 0.8941176470588234615, 0.8941176470588234615 ) ;
#2357 = PLANE ( 'NONE',  #4716 ) ;
#2358 = ORIENTED_EDGE ( 'NONE', *, *, #794, .T. ) ;
#2359 = SHAPE_DEFINITION_REPRESENTATION ( #10327, #9523 ) ;
#2360 = CARTESIAN_POINT ( 'NONE',  ( 19.40000000000002700, 62.98000740192551206, 2.937500001229034208 ) ) ;
#2361 = ORIENTED_EDGE ( 'NONE', *, *, #10556, .T. ) ;
#2362 = CARTESIAN_POINT ( 'NONE',  ( 34.49999999999998579, 96.48074069840785683, 22.38477631085024555 ) ) ;
#2363 = ORIENTED_EDGE ( 'NONE', *, *, #11691, .T. ) ;
#2364 = EDGE_CURVE ( 'NONE', #6336, #8478, #7652, .T. ) ;
#2365 = CARTESIAN_POINT ( 'NONE',  ( 38.50000000000000000, 90.00000000000000000, -3.000000000000000000 ) ) ;
#2366 = EDGE_CURVE ( 'NONE', #10005, #8267, #6599, .T. ) ;
#2367 = DIRECTION ( 'NONE',  ( 0.000000000000000000, 0.000000000000000000, 1.000000000000000000 ) ) ;
#2368 = CIRCLE ( 'NONE', #7365, 3.350000000000000089 ) ;
#2369 = DIRECTION ( 'NONE',  ( -0.5877852522924710277, 0.8090169943749490056, 0.000000000000000000 ) ) ;
#2370 = EDGE_CURVE ( 'NONE', #11848, #9339, #5779, .T. ) ;
#2371 = DIRECTION ( 'NONE',  ( 0.000000000000000000, 0.000000000000000000, 1.000000000000000000 ) ) ;
#2372 = ORIENTED_EDGE ( 'NONE', *, *, #10388, .F. ) ;
#2373 = DIRECTION ( 'NONE',  ( -0.3420201803727477285, 0.9396926073018736503, 0.000000000000000000 ) ) ;
#2374 = ORIENTED_EDGE ( 'NONE', *, *, #8330, .F. ) ;
#2375 = DIRECTION ( 'NONE',  ( -1.000000000000000000, 0.000000000000000000, -0.000000000000000000 ) ) ;
#2376 = ORIENTED_EDGE ( 'NONE', *, *, #5336, .F. ) ;
#2377 = PRESENTATION_LAYER_ASSIGNMENT (  '', '', ( #2579 ) ) ;
#2378 = VERTEX_POINT ( 'NONE', #738 ) ;
#2379 = PLANE ( 'NONE',  #5446 ) ;
#2380 = VECTOR ( 'NONE', #7304, 1000.000000000000000 ) ;
#2381 = CARTESIAN_POINT ( 'NONE',  ( 1.269999999999999796, 0.000000000000000000, 0.000000000000000000 ) ) ;
#2382 = ADVANCED_FACE ( 'NONE', ( #9770 ), #6819, .F. ) ;
#2383 = CARTESIAN_POINT ( 'NONE',  ( 3.556430356250015024, 90.00000000000000000, 3.959375000614517415 ) ) ;
#2384 = CARTESIAN_POINT ( 'NONE',  ( 1.436050757534458100, -5.516136167806656943, -0.8000000000000000444 ) ) ;
#2385 = FACE_OUTER_BOUND ( 'NONE', #7262, .T. ) ;
#2386 = LINE ( 'NONE', #12588, #12100 ) ;
#2387 = CARTESIAN_POINT ( 'NONE',  ( 41.00904217445251732, 92.47818727009297390, 22.38477631085024555 ) ) ;
#2388 = CIRCLE ( 'NONE', #12400, 31.19999999999999218 ) ;
#2389 = DIRECTION ( 'NONE',  ( 0.000000000000000000, 0.000000000000000000, -1.000000000000000000 ) ) ;
#2390 = FACE_OUTER_BOUND ( 'NONE', #12019, .T. ) ;
#2391 = DIRECTION ( 'NONE',  ( -0.000000000000000000, 1.000000000000000000, -0.000000000000000000 ) ) ;
#2392 = AXIS2_PLACEMENT_3D ( 'NONE', #7373, #8364, #4435 ) ;
#2393 = LINE ( 'NONE', #211, #2946 ) ;
#2394 = DIRECTION ( 'NONE',  ( 1.000000000000000000, 2.135044278125301343E-15, 0.000000000000000000 ) ) ;
#2395 = ORIENTED_EDGE ( 'NONE', *, *, #2605, .F. ) ;
#2396 = ADVANCED_FACE ( 'NONE', ( #3762 ), #7744, .T. ) ;
#2397 = DIRECTION ( 'NONE',  ( 0.000000000000000000, -1.000000000000000000, 0.000000000000000000 ) ) ;
#2398 = VERTEX_POINT ( 'NONE', #12911 ) ;
#2399 = PRODUCT_DEFINITION_SHAPE ( 'NONE', 'NONE',  #8014 ) ;
#2400 = EDGE_CURVE ( 'NONE', #12580, #11762, #8278, .T. ) ;
#2401 = VECTOR ( 'NONE', #6897, 1000.000000000000000 ) ;
#2402 = CARTESIAN_POINT ( 'NONE',  ( 2.387319993259524598, -4.036502139894371233, -0.8000000000000000444 ) ) ;
#2403 = LINE ( 'NONE', #5775, #8274 ) ;
#2404 = EDGE_CURVE ( 'NONE', #10269, #7344, #860, .T. ) ;
#2405 = PLANE ( 'NONE',  #4057 ) ;
#2406 = EDGE_CURVE ( 'NONE', #11844, #11880, #12868, .T. ) ;
#2407 = ORIENTED_EDGE ( 'NONE', *, *, #1637, .F. ) ;
#2408 = CIRCLE ( 'NONE', #1347, 2.849999999999999645 ) ;
#2409 = DIRECTION ( 'NONE',  ( 0.000000000000000000, 0.000000000000000000, -1.000000000000000000 ) ) ;
#2410 = DIRECTION ( 'NONE',  ( -0.000000000000000000, -0.000000000000000000, -1.000000000000000000 ) ) ;
#2411 = AXIS2_PLACEMENT_3D ( 'NONE', #1068, #9183, #339 ) ;
#2412 = EDGE_LOOP ( 'NONE', ( #6661, #9476, #10070 ) ) ;
#2413 = DIRECTION ( 'NONE',  ( -1.000000000000000000, 0.000000000000000000, 0.000000000000000000 ) ) ;
#2414 = ORIENTED_EDGE ( 'NONE', *, *, #10673, .T. ) ;
#2415 = ORIENTED_EDGE ( 'NONE', *, *, #9712, .F. ) ;
#2416 = CARTESIAN_POINT ( 'NONE',  ( 1.040000000000000036, 1.154700538379252350, -1.084202172485497162E-16 ) ) ;
#2417 = DIRECTION ( 'NONE',  ( -0.000000000000000000, -0.5000000000000000000, 0.8660254037844385966 ) ) ;
#2418 = AXIS2_PLACEMENT_3D ( 'NONE', #6060, #956, #2016 ) ;
#2419 = VERTEX_POINT ( 'NONE', #4990 ) ;
#2420 = PRODUCT_DEFINITION_CONTEXT ( 'detailed design', #7683, 'design' ) ;
#2421 = CIRCLE ( 'NONE', #11603, 1.500000000000002665 ) ;
#2422 = SHAPE_REPRESENTATION ( 'support', ( #5704 ), #466 ) ;
#2423 = VERTEX_POINT ( 'NONE', #11987 ) ;
#2424 = DIRECTION ( 'NONE',  ( -1.000000000000000000, 0.000000000000000000, 0.000000000000000000 ) ) ;
#2425 = ORIENTED_EDGE ( 'NONE', *, *, #7142, .T. ) ;
#2426 = DIRECTION ( 'NONE',  ( 1.000000000000000000, 0.000000000000000000, 5.337610695313252124E-17 ) ) ;
#2427 = CARTESIAN_POINT ( 'NONE',  ( 3.800000000000015365, 90.00000000000000000, 4.212500001229034119 ) ) ;
#2428 = ORIENTED_EDGE ( 'NONE', *, *, #841, .F. ) ;
#2429 = CIRCLE ( 'NONE', #9729, 31.20000000000000284 ) ;
#2430 = EDGE_CURVE ( 'NONE', #7384, #7875, #11194, .T. ) ;
#2431 = DIRECTION ( 'NONE',  ( 0.000000000000000000, 0.000000000000000000, 1.000000000000000000 ) ) ;
#2432 = ORIENTED_EDGE ( 'NONE', *, *, #4273, .F. ) ;
#2433 = VECTOR ( 'NONE', #12944, 1000.000000000000000 ) ;
#2434 = DIRECTION ( 'NONE',  ( -0.000000000000000000, 0.5000000000000003331, 0.8660254037844384856 ) ) ;
#2435 = ORIENTED_EDGE ( 'NONE', *, *, #4012, .T. ) ;
#2436 = LINE ( 'NONE', #9227, #6096 ) ;
#2437 = DIRECTION ( 'NONE',  ( 0.000000000000000000, 0.000000000000000000, 1.000000000000000000 ) ) ;
#2438 = FILL_AREA_STYLE_COLOUR ( '', #6750 ) ;
#2439 = ORIENTED_EDGE ( 'NONE', *, *, #6829, .T. ) ;
#2440 = CIRCLE ( 'NONE', #4313, 1.219500000000000028 ) ;
#2441 = CARTESIAN_POINT ( 'NONE',  ( 64.43284985331906967, 100.7126819209670145, 2.929163888449521025 ) ) ;
#2442 = ORIENTED_EDGE ( 'NONE', *, *, #10214, .T. ) ;
#2443 = DIRECTION ( 'NONE',  ( 0.000000000000000000, -1.000000000000000000, 0.000000000000000000 ) ) ;
#2444 = CARTESIAN_POINT ( 'NONE',  ( 66.44356964374999563, 90.00000000000000000, 3.734375000614516882 ) ) ;
#2445 = EDGE_CURVE ( 'NONE', #11236, #5069, #2909, .T. ) ;
#2446 = EDGE_LOOP ( 'NONE', ( #162, #3575, #4707, #65 ) ) ;
#2447 = LINE ( 'NONE', #12380, #9210 ) ;
#2448 = CARTESIAN_POINT ( 'NONE',  ( 34.25000000000000000, 92.49999999999998579, 6.000000000000000000 ) ) ;
#2449 = VECTOR ( 'NONE', #8607, 1000.000000000000114 ) ;
#2450 = CARTESIAN_POINT ( 'NONE',  ( 35.00000000000000000, 126.3079067962036106, 3.846875000614517592 ) ) ;
#2451 = DIRECTION ( 'NONE',  ( -0.000000000000000000, 1.000000000000000000, -0.000000000000000000 ) ) ;
#2452 = DIRECTION ( 'NONE',  ( 0.000000000000000000, 0.000000000000000000, 1.000000000000000000 ) ) ;
#2453 = CARTESIAN_POINT ( 'NONE',  ( 7.573869524628007888, 99.43702109502098097, 4.000000000000000000 ) ) ;
#2454 = DIRECTION ( 'NONE',  ( -0.3262398754384822630, 0.9452870165584014162, 0.000000000000000000 ) ) ;
#2455 = EDGE_CURVE ( 'NONE', #8074, #6272, #11131, .T. ) ;
#2456 = DIRECTION ( 'NONE',  ( -1.000000000000000000, 0.000000000000000000, -0.000000000000000000 ) ) ;
#2457 = DIRECTION ( 'NONE',  ( 0.000000000000000000, 1.000000000000000000, 0.000000000000000000 ) ) ;
#2458 = AXIS2_PLACEMENT_3D ( 'NONE', #11881, #2008, #10893 ) ;
#2459 = DIRECTION ( 'NONE',  ( 0.000000000000000000, 0.000000000000000000, 1.000000000000000000 ) ) ;
#2460 = LINE ( 'NONE', #4229, #4608 ) ;
#2461 = DIRECTION ( 'NONE',  ( 0.000000000000000000, 0.000000000000000000, 1.000000000000000000 ) ) ;
#2462 = ORIENTED_EDGE ( 'NONE', *, *, #7361, .T. ) ;
#2463 = DIRECTION ( 'NONE',  ( -0.000000000000000000, 1.000000000000000000, -0.000000000000000000 ) ) ;
#2464 = LINE ( 'NONE', #2660, #12900 ) ;
#2465 = ORIENTED_EDGE ( 'NONE', *, *, #12549, .F. ) ;
#2466 = CONICAL_SURFACE ( 'NONE', #12491, 1.219500000000000028, 0.7853981633974487231 ) ;
#2467 =( NAMED_UNIT ( * ) PLANE_ANGLE_UNIT ( ) SI_UNIT ( $, .RADIAN. ) );
#2468 = CARTESIAN_POINT ( 'NONE',  ( -57.99999999999999289, 30.00000000000000000, 7.999999999999996447 ) ) ;
#2469 = ADVANCED_FACE ( 'NONE', ( #1920 ), #5901, .F. ) ;
#2470 = CARTESIAN_POINT ( 'NONE',  ( 25.00000000000000355, -5.000000000000000000, -4.249999999999998224 ) ) ;
#2471 = VERTEX_POINT ( 'NONE', #5182 ) ;
#2472 = CARTESIAN_POINT ( 'NONE',  ( 0.000000000000000000, -1.154700538379251240, 1.014316938424154191E-17 ) ) ;
#2473 = CARTESIAN_POINT ( 'NONE',  ( 66.44356964374998142, 108.1539533981018053, 4.615625000614516971 ) ) ;
#2474 = AXIS2_PLACEMENT_3D ( 'NONE', #7848, #1706, #7658 ) ;
#2475 = ORIENTED_EDGE ( 'NONE', *, *, #7794, .F. ) ;
#2476 = SURFACE_STYLE_USAGE ( .BOTH. , #3333 ) ;
#2477 = CARTESIAN_POINT ( 'NONE',  ( -57.99999999999999289, 30.00000000000000000, 0.000000000000000000 ) ) ;
#2478 = EDGE_LOOP ( 'NONE', ( #5655, #9956 ) ) ;
#2479 = CARTESIAN_POINT ( 'NONE',  ( -60.00000000000000000, 30.00000000000000000, -1.000000000000000000 ) ) ;
#2480 = ORIENTED_EDGE ( 'NONE', *, *, #8048, .T. ) ;
#2481 = EDGE_CURVE ( 'NONE', #2101, #4251, #4211, .T. ) ;
#2482 = LINE ( 'NONE', #4701, #10293 ) ;
#2483 = CARTESIAN_POINT ( 'NONE',  ( 4.336808689942017736E-16, -1.425000000000000044, -2.617682533177466553E-16 ) ) ;
#2484 = VERTEX_POINT ( 'NONE', #131 ) ;
#2485 = VECTOR ( 'NONE', #6651, 1000.000000000000000 ) ;
#2486 = CARTESIAN_POINT ( 'NONE',  ( 1.040000000000000036, -0.5773502691896253980, 1.000000000000000000 ) ) ;
#2487 = DIRECTION ( 'NONE',  ( 0.000000000000000000, 0.000000000000000000, 1.000000000000000000 ) ) ;
#2488 = ORIENTED_EDGE ( 'NONE', *, *, #12869, .T. ) ;
#2489 = ADVANCED_FACE ( 'NONE', ( #12122 ), #259, .T. ) ;
#2490 = CARTESIAN_POINT ( 'NONE',  ( 45.00000000000000000, 0.000000000000000000, -5.750000000000000000 ) ) ;
#2491 = SHAPE_DEFINITION_REPRESENTATION ( #6355, #7342 ) ;
#2492 = CARTESIAN_POINT ( 'NONE',  ( 35.00000000000000711, 53.97334320256736362, 2.975000001229034741 ) ) ;
#2493 = EDGE_LOOP ( 'NONE', ( #12356, #6274 ) ) ;
#2494 = FACE_OUTER_BOUND ( 'NONE', #11714, .T. ) ;
#2495 = ORIENTED_EDGE ( 'NONE', *, *, #1293, .F. ) ;
#2496 = VECTOR ( 'NONE', #1304, 1000.000000000000114 ) ;
#2497 = ORIENTED_EDGE ( 'NONE', *, *, #1962, .T. ) ;
#2498 = ADVANCED_FACE ( 'NONE', ( #3366, #195 ), #2118, .T. ) ;
#2499 = CARTESIAN_POINT ( 'NONE',  ( 20.61329739217925194, 62.19155013526994935, 3.000000000000000444 ) ) ;
#2500 = FACE_OUTER_BOUND ( 'NONE', #5926, .T. ) ;
#2501 = VECTOR ( 'NONE', #6851, 1000.000000000000000 ) ;
#2502 = CONICAL_SURFACE ( 'NONE', #9807, 1732.050807568857181, 1.047197551196592746 ) ;
#2503 = ORIENTED_EDGE ( 'NONE', *, *, #9032, .T. ) ;
#2504 = CARTESIAN_POINT ( 'NONE',  ( 19.27821517812500574, 117.2309300971526937, 3.884375000614516793 ) ) ;
#2505 = ORIENTED_EDGE ( 'NONE', *, *, #3170, .T. ) ;
#2506 = CARTESIAN_POINT ( 'NONE',  ( 50.59999999999999432, 117.0199925980744666, 3.162500001229034741 ) ) ;
#2507 = VERTEX_POINT ( 'NONE', #2254 ) ;
#2508 = CARTESIAN_POINT ( 'NONE',  ( 35.00000000000000000, 126.3079067962035822, 4.296875000614517326 ) ) ;
#2509 = PRODUCT_DEFINITION_SHAPE ( 'NONE', 'NONE',  #8584 ) ;
#2510 = ORIENTED_EDGE ( 'NONE', *, *, #1576, .F. ) ;
#2511 = AXIS2_PLACEMENT_3D ( 'NONE', #6884, #5777, #9767 ) ;
#2512 = CARTESIAN_POINT ( 'NONE',  ( 64.85903780527353035, 87.09520029206045422, 1.000000000000003553 ) ) ;
#2513 = CARTESIAN_POINT ( 'NONE',  ( 3.556430356250028790, 71.84604660189818048, 3.096875000614517148 ) ) ;
#2514 = CARTESIAN_POINT ( 'NONE',  ( 50.72178482187501203, 62.76906990284730625, 4.503125000614517148 ) ) ;
#2515 = APPLICATION_CONTEXT ( 'automotive_design' ) ;
#2516 = FACE_OUTER_BOUND ( 'NONE', #10675, .T. ) ;
#2517 = LINE ( 'NONE', #8403, #1013 ) ;
#2518 = EDGE_CURVE ( 'NONE', #8071, #9176, #6094, .T. ) ;
#2519 = VECTOR ( 'NONE', #1349, 1000.000000000000000 ) ;
#2520 = CARTESIAN_POINT ( 'NONE',  ( -53.07079676972452376, 33.99826794919245998, -1.000000000000000000 ) ) ;
#2521 = PLANE ( 'NONE',  #10430 ) ;
#2522 = CARTESIAN_POINT ( 'NONE',  ( -48.33333333333332860, 0.000000000000000000, -1.734723475976807094E-15 ) ) ;
#2523 = DIRECTION ( 'NONE',  ( 0.000000000000000000, -0.000000000000000000, -1.000000000000000000 ) ) ;
#2524 = CARTESIAN_POINT ( 'NONE',  ( 66.20000000000005969, 108.0133283987162685, 4.812499999999999112 ) ) ;
#2525 = CARTESIAN_POINT ( 'NONE',  ( 35.00000000000000000, 90.00000000000000000, 4.000000000000000000 ) ) ;
#2526 = ORIENTED_EDGE ( 'NONE', *, *, #6460, .T. ) ;
#2527 = DIRECTION ( 'NONE',  ( -1.000000000000000000, -0.000000000000000000, -0.000000000000000000 ) ) ;
#2528 = AXIS2_PLACEMENT_3D ( 'NONE', #6434, #12203, #4480 ) ;
#2529 = DIRECTION ( 'NONE',  ( 1.000000000000000000, 0.000000000000000000, 0.000000000000000000 ) ) ;
#2530 = ORIENTED_EDGE ( 'NONE', *, *, #6268, .T. ) ;
#2531 = ADVANCED_FACE ( 'NONE', ( #8070 ), #7146, .F. ) ;
#2532 = EDGE_CURVE ( 'NONE', #4396, #427, #3068, .T. ) ;
#2533 = CARTESIAN_POINT ( 'NONE',  ( 50.00000000000000000, 2.000000000000000000, 10.00000000000000000 ) ) ;
#2534 = CARTESIAN_POINT ( 'NONE',  ( -60.00000000000000000, 30.00000000000000000, 2.500000000000000000 ) ) ;
#2535 = PLANE ( 'NONE',  #66 ) ;
#2536 = VECTOR ( 'NONE', #10878, 1000.000000000000000 ) ;
#2537 = ORIENTED_EDGE ( 'NONE', *, *, #6254, .T. ) ;
#2538 = DIRECTION ( 'NONE',  ( -0.8660254037844359321, -0.5000000000000046629, -0.000000000000000000 ) ) ;
#2539 = DIRECTION ( 'NONE',  ( 0.000000000000000000, 0.000000000000000000, -1.000000000000000000 ) ) ;
#2540 = ORIENTED_EDGE ( 'NONE', *, *, #11563, .T. ) ;
#2541 = CARTESIAN_POINT ( 'NONE',  ( -53.33333333333332149, 36.15840287135605990, 1.000000000000000888 ) ) ;
#2542 = ORIENTED_EDGE ( 'NONE', *, *, #349, .F. ) ;
#2543 = VERTEX_POINT ( 'NONE', #2052 ) ;
#2544 = ADVANCED_FACE ( 'NONE', ( #8266 ), #7216, .T. ) ;
#2545 = CARTESIAN_POINT ( 'NONE',  ( 8.500000000000000000, 69.54849343948981755, 2.999999999999918288 ) ) ;
#2546 = CIRCLE ( 'NONE', #431, 3.500000000000003109 ) ;
#2547 = CARTESIAN_POINT ( 'NONE',  ( 1.040000000000000036, 0.5773502691896263972, 1.000000000000000000 ) ) ;
#2548 = EDGE_LOOP ( 'NONE', ( #8498, #47, #12554, #10610 ) ) ;
#2549 = DIRECTION ( 'NONE',  ( -1.000000000000000000, -0.000000000000000000, -0.000000000000000000 ) ) ;
#2550 = FACE_OUTER_BOUND ( 'NONE', #5796, .T. ) ;
#2551 = CARTESIAN_POINT ( 'NONE',  ( 35.00000000000000000, 90.00000000000000000, -0.9999999999999970024 ) ) ;
#2552 = ORIENTED_EDGE ( 'NONE', *, *, #8701, .F. ) ;
#2553 = DIRECTION ( 'NONE',  ( -0.5000000000000045519, 0.8660254037844360431, 0.000000000000000000 ) ) ;
#2554 = CARTESIAN_POINT ( 'NONE',  ( 35.00000000000000711, 53.97334320256736362, 3.425000001229034474 ) ) ;
#2555 = ORIENTED_EDGE ( 'NONE', *, *, #5643, .F. ) ;
#2556 = PRESENTATION_LAYER_ASSIGNMENT (  '', '', ( #1070 ) ) ;
#2557 = FACE_OUTER_BOUND ( 'NONE', #5571, .T. ) ;
#2558 = ORIENTED_EDGE ( 'NONE', *, *, #2882, .F. ) ;
#2559 = EDGE_LOOP ( 'NONE', ( #102, #5637, #7763, #11235 ) ) ;
#2560 = ADVANCED_FACE ( 'NONE', ( #6162 ), #7343, .F. ) ;
#2561 = CARTESIAN_POINT ( 'NONE',  ( 40.44561422048254684, 59.23121341156224418, 2.999999999999998668 ) ) ;
#2562 = CARTESIAN_POINT ( 'NONE',  ( 35.00000000000000000, 90.00000000000000000, -1.000000000000000000 ) ) ;
#2563 = AXIS2_PLACEMENT_3D ( 'NONE', #1848, #1719, #3692 ) ;
#2564 = ORIENTED_EDGE ( 'NONE', *, *, #10426, .F. ) ;
#2565 = CARTESIAN_POINT ( 'NONE',  ( 3.556430356250014579, 108.1539533981018053, 3.921875000614517326 ) ) ;
#2566 = ORIENTED_EDGE ( 'NONE', *, *, #6741, .F. ) ;
#2567 = EDGE_CURVE ( 'NONE', #12299, #11967, #8135, .T. ) ;
#2568 = DIRECTION ( 'NONE',  ( -1.000000000000000000, -0.000000000000000000, -0.000000000000000000 ) ) ;
#2569 = EDGE_CURVE ( 'NONE', #3421, #12815, #9041, .T. ) ;
#2570 = ORIENTED_EDGE ( 'NONE', *, *, #4635, .F. ) ;
#2571 = CARTESIAN_POINT ( 'NONE',  ( 19.27821517812503060, 62.76906990284727783, 3.134375000614517237 ) ) ;
#2572 = ORIENTED_EDGE ( 'NONE', *, *, #12077, .T. ) ;
#2573 = CARTESIAN_POINT ( 'NONE',  ( 35.00000000000000000, 90.00000000000000000, -3.799999999999999378 ) ) ;
#2574 = DIRECTION ( 'NONE',  ( -0.000000000000000000, -0.000000000000000000, 1.000000000000000000 ) ) ;
#2575 = CARTESIAN_POINT ( 'NONE',  ( 35.00000000000000000, 90.00000000000000000, 4.000000000000000000 ) ) ;
#2576 = FACE_OUTER_BOUND ( 'NONE', #10821, .T. ) ;
#2577 = CYLINDRICAL_SURFACE ( 'NONE', #10215, 10.00000000000000178 ) ;
#2578 = CARTESIAN_POINT ( 'NONE',  ( -65.00000000000004263, 38.66025403784436065, 3.000000000000000000 ) ) ;
#2579 = STYLED_ITEM ( 'NONE', ( #11547 ), #9016 ) ;
#2580 = CARTESIAN_POINT ( 'NONE',  ( 34.25000000000000000, 93.41869858279433458, 6.000000000000000000 ) ) ;
#2581 = LINE ( 'NONE', #6431, #1656 ) ;
#2582 = CARTESIAN_POINT ( 'NONE',  ( 1.599999999999999867, -4.873461295629625489, -0.8000000000000000444 ) ) ;
#2583 = VECTOR ( 'NONE', #3302, 1000.000000000000000 ) ;
#2584 = DIRECTION ( 'NONE',  ( 0.000000000000000000, 1.224646799147353207E-16, -1.000000000000000000 ) ) ;
#2585 = DIRECTION ( 'NONE',  ( -0.000000000000000000, 1.000000000000000000, -0.000000000000000000 ) ) ;
#2586 = DIRECTION ( 'NONE',  ( 1.000000000000000000, 0.000000000000000000, 0.000000000000000000 ) ) ;
#2587 = EDGE_CURVE ( 'NONE', #2398, #3791, #6541, .T. ) ;
#2588 = ORIENTED_EDGE ( 'NONE', *, *, #11621, .F. ) ;
#2590 = CARTESIAN_POINT ( 'NONE',  ( 3.800000000000025135, 71.98667160128366049, 3.237500000000000266 ) ) ;
#2589 = COLOUR_RGB ( '',0.8941176470588234615, 0.8941176470588234615, 0.8941176470588234615 ) ;
#2591 = CARTESIAN_POINT ( 'NONE',  ( -48.33333333333332860, 2.000000000000001332, -1.734723475976807094E-15 ) ) ;
#2592 = ORIENTED_EDGE ( 'NONE', *, *, #7347, .F. ) ;
#2593 = AXIS2_PLACEMENT_3D ( 'NONE', #4042, #8031, #7044 ) ;
#2594 = CARTESIAN_POINT ( 'NONE',  ( -31.49999999999998579, 48.76388374866304076, 1.000000000000000000 ) ) ;
#2595 = FACE_OUTER_BOUND ( 'NONE', #6007, .T. ) ;
#2596 = CARTESIAN_POINT ( 'NONE',  ( 1.625004804578465745, -6.241943558307532669, 0.000000000000000000 ) ) ;
#2597 = ORIENTED_EDGE ( 'NONE', *, *, #1654, .F. ) ;
#2598 = EDGE_CURVE ( 'NONE', #1585, #3338, #2319, .T. ) ;
#2599 = CARTESIAN_POINT ( 'NONE',  ( -61.88397459621560870, 33.26313972081441506, 1.836970198721030427E-16 ) ) ;
#2600 = FACE_OUTER_BOUND ( 'NONE', #10043, .T. ) ;
#2601 = EDGE_LOOP ( 'NONE', ( #4533, #2070, #7751, #6048 ) ) ;
#2602 = DIRECTION ( 'NONE',  ( 0.5000000000000049960, -0.8660254037844357100, 0.000000000000000000 ) ) ;
#2603 = CIRCLE ( 'NONE', #9700, 1.000000000000000000 ) ;
#2604 = DIRECTION ( 'NONE',  ( -0.000000000000000000, -0.000000000000000000, -1.000000000000000000 ) ) ;
#2605 = EDGE_CURVE ( 'NONE', #3551, #10547, #11766, .T. ) ;
#2606 = ORIENTED_EDGE ( 'NONE', *, *, #3931, .T. ) ;
#2607 = VECTOR ( 'NONE', #5725, 1000.000000000000000 ) ;
#2608 = CARTESIAN_POINT ( 'NONE',  ( 35.00000000000000000, 90.00000000000000000, 5.000000000000000000 ) ) ;
#2609 = ORIENTED_EDGE ( 'NONE', *, *, #9479, .F. ) ;
#2610 = FACE_OUTER_BOUND ( 'NONE', #7322, .T. ) ;
#2611 = DIRECTION ( 'NONE',  ( -1.000000000000000000, -0.000000000000000000, -0.000000000000000000 ) ) ;
#2612 = DIRECTION ( 'NONE',  ( 0.000000000000000000, 0.000000000000000000, -1.000000000000000000 ) ) ;
#2613 = AXIS2_PLACEMENT_3D ( 'NONE', #8406, #9578, #12389 ) ;
#2614 = ORIENTED_EDGE ( 'NONE', *, *, #7142, .F. ) ;
#2615 = VECTOR ( 'NONE', #3758, 1000.000000000000000 ) ;
#2616 = CARTESIAN_POINT ( 'NONE',  ( 9.999999999999994671, 27.00000000000000000, 2.500000000000000000 ) ) ;
#2617 = ORIENTED_EDGE ( 'NONE', *, *, #10476, .F. ) ;
#2618 = DIRECTION ( 'NONE',  ( 0.8090169943749456749, -0.5877852522924754686, 0.000000000000000000 ) ) ;
#2619 = PRODUCT_CONTEXT ( 'NONE', #12365, 'mechanical' ) ;
#2620 = CARTESIAN_POINT ( 'NONE',  ( 50.60000000000001563, 62.98000740192552627, 3.912500001229034297 ) ) ;
#2621 = ADVANCED_FACE ( 'NONE', ( #8331 ), #1056, .F. ) ;
#2622 = ORIENTED_EDGE ( 'NONE', *, *, #3607, .F. ) ;
#2623 = FACE_OUTER_BOUND ( 'NONE', #6598, .T. ) ;
#2624 = ORIENTED_EDGE ( 'NONE', *, *, #8393, .T. ) ;
#2625 = CARTESIAN_POINT ( 'NONE',  ( 35.75000000000000711, 92.49999999999998579, -8.000000000000000000 ) ) ;
#2627 = VERTEX_POINT ( 'NONE', #6486 ) ;
#2626 = AXIS2_PLACEMENT_3D ( 'NONE', #11682, #4497, #10508 ) ;
#2628 = VECTOR ( 'NONE', #10063, 1000.000000000000000 ) ;
#2629 = CARTESIAN_POINT ( 'NONE',  ( 4.785832313128271842, 81.33916431800814451, 2.999999999999999112 ) ) ;
#2630 = LINE ( 'NONE', #3357, #2896 ) ;
#2631 = EDGE_LOOP ( 'NONE', ( #8821, #12095, #8765, #147 ) ) ;
#2632 = CARTESIAN_POINT ( 'NONE',  ( 66.44356964374998142, 108.1539533981018053, 4.221875000614517148 ) ) ;
#2633 = ORIENTED_EDGE ( 'NONE', *, *, #1361, .T. ) ;
#2634 = VECTOR ( 'NONE', #12268, 1000.000000000000000 ) ;
#2635 = PLANE ( 'NONE',  #6877 ) ;
#2636 = EDGE_CURVE ( 'NONE', #6649, #7180, #12447, .T. ) ;
#2637 = AXIS2_PLACEMENT_3D ( 'NONE', #9130, #12147, #10308 ) ;
#2638 = ORIENTED_EDGE ( 'NONE', *, *, #4093, .F. ) ;
#2639 = ADVANCED_BREP_SHAPE_REPRESENTATION ( '', ( #3242, #5704 ), #11354 ) ;
#2640 = CARTESIAN_POINT ( 'NONE',  ( 19.27821517812500574, 117.2309300971526937, 3.434375000614517059 ) ) ;
#2641 = ORIENTED_EDGE ( 'NONE', *, *, #9032, .F. ) ;
#2642 = DIRECTION ( 'NONE',  ( -0.8660254037844360431, -0.5000000000000047740, -0.000000000000000000 ) ) ;
#2643 = CARTESIAN_POINT ( 'NONE',  ( 50.59999999999999432, 117.0199925980744666, 3.050000000000000266 ) ) ;
#2644 = DIRECTION ( 'NONE',  ( 0.9510565162951528650, 0.3090169943749500048, 0.000000000000000000 ) ) ;
#2645 = CYLINDRICAL_SURFACE ( 'NONE', #11019, 0.7500000000000000000 ) ;
#2646 = AXIS2_PLACEMENT_3D ( 'NONE', #7873, #6756, #799 ) ;
#2647 = ADVANCED_FACE ( 'NONE', ( #1385 ), #11076, .T. ) ;
#2648 = ADVANCED_FACE ( 'NONE', ( #8900, #3940 ), #11718, .F. ) ;
#2649 = CARTESIAN_POINT ( 'NONE',  ( 52.45028081366923089, 66.83239978927284142, -1.000000000000000000 ) ) ;
#2650 = CYLINDRICAL_SURFACE ( 'NONE', #8253, 3.499999999999996003 ) ;
#2651 = DIRECTION ( 'NONE',  ( 0.000000000000000000, 0.000000000000000000, 1.000000000000000000 ) ) ;
#2652 = DIRECTION ( 'NONE',  ( 0.000000000000000000, 0.000000000000000000, -1.000000000000000000 ) ) ;
#2653 = EDGE_CURVE ( 'NONE', #11634, #5783, #6740, .T. ) ;
#2654 = DIRECTION ( 'NONE',  ( 0.8660254037844361541, 0.5000000000000045519, -0.000000000000000000 ) ) ;
#2655 = VECTOR ( 'NONE', #11610, 1000.000000000000000 ) ;
#2656 = LINE ( 'NONE', #2720, #10467 ) ;
#2657 = CARTESIAN_POINT ( 'NONE',  ( 35.00000000000000000, 126.0266567974326222, 3.650000001229033675 ) ) ;
#2658 = ORIENTED_EDGE ( 'NONE', *, *, #1813, .T. ) ;
#2659 = CARTESIAN_POINT ( 'NONE',  ( 19.40000000000000924, 117.0199925980744666, 4.025000000000000355 ) ) ;
#2660 = CARTESIAN_POINT ( 'NONE',  ( 31.50000000000000000, 90.00000000000000000, 6.000000000000000000 ) ) ;
#2661 = ORIENTED_EDGE ( 'NONE', *, *, #10729, .F. ) ;
#2662 = AXIS2_PLACEMENT_3D ( 'NONE', #818, #1938, #3975 ) ;
#2663 = CARTESIAN_POINT ( 'NONE',  ( 19.89999999999999858, 90.00000000000000000, -10.00000000000000178 ) ) ;
#2664 = ADVANCED_FACE ( 'NONE', ( #5766, #10068, #4131, #7131, #4261, #8118, #10135 ), #11184, .T. ) ;
#2665 = CARTESIAN_POINT ( 'NONE',  ( 20.00000000000000355, 0.000000000000000000, 10.00000000000000000 ) ) ;
#2666 = VERTEX_POINT ( 'NONE', #11048 ) ;
#2667 = CARTESIAN_POINT ( 'NONE',  ( 1.040000000000000036, 1.154700538379252350, 7.017607234860990640E-28 ) ) ;
#2668 = CARTESIAN_POINT ( 'NONE',  ( 19.27821517812500574, 117.2309300971526937, 3.828125000614516882 ) ) ;
#2669 = FACE_OUTER_BOUND ( 'NONE', #1773, .T. ) ;
#2670 = FACE_OUTER_BOUND ( 'NONE', #3257, .T. ) ;
#2671 = ORIENTED_EDGE ( 'NONE', *, *, #1841, .T. ) ;
#2672 = AXIS2_PLACEMENT_3D ( 'NONE', #5721, #7947, #2977 ) ;
#2673 = CARTESIAN_POINT ( 'NONE',  ( 50.59999999999999432, 117.0199925980744666, 4.400000000000000355 ) ) ;
#2674 = ORIENTED_EDGE ( 'NONE', *, *, #8986, .T. ) ;
#2675 = FACE_OUTER_BOUND ( 'NONE', #12632, .T. ) ;
#2676 = CARTESIAN_POINT ( 'NONE',  ( 1.040000000000000036, 0.000000000000000000, 2.000000000000000000 ) ) ;
#2677 = CARTESIAN_POINT ( 'NONE',  ( 1.040000000000000036, -1.154700538379251684, -1.199226976249124676E-17 ) ) ;
#2678 = ADVANCED_FACE ( 'NONE', ( #3218 ), #12170, .T. ) ;
#2679 = ORIENTED_EDGE ( 'NONE', *, *, #10729, .T. ) ;
#2680 = CIRCLE ( 'NONE', #11656, 3.500000000000003109 ) ;
#2681 = DIRECTION ( 'NONE',  ( -1.914177628664063178E-15, 1.000000000000000000, 0.000000000000000000 ) ) ;
#2682 = EDGE_LOOP ( 'NONE', ( #9674, #629, #7586, #5744 ) ) ;
#2683 = DIRECTION ( 'NONE',  ( -0.000000000000000000, -0.000000000000000000, -1.000000000000000000 ) ) ;
#2684 = LINE ( 'NONE', #1949, #10025 ) ;
#2685 = ORIENTED_EDGE ( 'NONE', *, *, #3331, .T. ) ;
#2686 = B_SPLINE_CURVE_WITH_KNOTS ( 'NONE', 3,
 ( #10985, #6874, #10072, #8963 ),
 .UNSPECIFIED., .F., .F.,
 ( 4, 4 ),
 ( 0.000000000000000000, 0.5999999999999995337 ),
 .UNSPECIFIED. ) ;
#2687 = SURFACE_STYLE_FILL_AREA ( #1635 ) ;
#2688 = EDGE_LOOP ( 'NONE', ( #10332, #2797, #7879, #9218, #1446, #2784, #5155, #2606, #1761, #1842, #1195 ) ) ;
#2689 = CARTESIAN_POINT ( 'NONE',  ( 33.50000000000000711, 67.79999999999999716, 8.000000000000000000 ) ) ;
#2690 = ORIENTED_EDGE ( 'NONE', *, *, #5106, .F. ) ;
#2691 = AXIS2_PLACEMENT_3D ( 'NONE', #3323, #6315, #2277 ) ;
#2692 = AXIS2_PLACEMENT_3D ( 'NONE', #1032, #9211, #1164 ) ;
#2693 = DIRECTION ( 'NONE',  ( 0.000000000000000000, 0.000000000000000000, -1.000000000000000000 ) ) ;
#2694 = CARTESIAN_POINT ( 'NONE',  ( 35.49999999999999289, 96.48074069840785683, 4.000000000000000000 ) ) ;
#2695 = EDGE_CURVE ( 'NONE', #12353, #5750, #10666, .T. ) ;
#2696 = UNCERTAINTY_MEASURE_WITH_UNIT (LENGTH_MEASURE( 1.000000000000000082E-05 ), #163, 'distance_accuracy_value', 'NONE');
#2697 = EDGE_CURVE ( 'NONE', #8362, #12765, #2102, .T. ) ;
#2698 = ORIENTED_EDGE ( 'NONE', *, *, #7886, .T. ) ;
#2699 = CARTESIAN_POINT ( 'NONE',  ( 52.49999999999996447, 86.00000000000000000, -8.000000000000000000 ) ) ;
#2700 = ORIENTED_EDGE ( 'NONE', *, *, #10576, .F. ) ;
#2701 = CARTESIAN_POINT ( 'NONE',  ( 50.60000000000001563, 62.98000740192552627, 3.012500001229034829 ) ) ;
#2702 = AXIS2_PLACEMENT_3D ( 'NONE', #6364, #3178, #7225 ) ;
#2703 = ORIENTED_EDGE ( 'NONE', *, *, #5308, .F. ) ;
#2704 = CARTESIAN_POINT ( 'NONE',  ( 3.556430356250028790, 71.84604660189818048, 3.490625000614517415 ) ) ;
#2705 = ORIENTED_EDGE ( 'NONE', *, *, #9543, .T. ) ;
#2706 = DIRECTION ( 'NONE',  ( 4.336808689942017736E-16, 2.503857664561960972E-16, 1.000000000000000000 ) ) ;
#2707 = CARTESIAN_POINT ( 'NONE',  ( 60.43447303579327468, 111.3420569435211149, 3.026359439817805086 ) ) ;
#2708 = LINE ( 'NONE', #12109, #3815 ) ;
#2709 = VECTOR ( 'NONE', #6817, 1000.000000000000000 ) ;
#2710 = CARTESIAN_POINT ( 'NONE',  ( 35.00000000000000711, 53.69209320379640360, 3.565625000614517592 ) ) ;
#2711 = ADVANCED_FACE ( 'NONE', ( #2036 ), #5165, .F. ) ;
#2712 = CIRCLE ( 'NONE', #3755, 1.599999999999997202 ) ;
#2713 = CYLINDRICAL_SURFACE ( 'NONE', #3339, 31.19999999999998863 ) ;
#2714 = CARTESIAN_POINT ( 'NONE',  ( 35.00000000000000711, 53.97334320256736362, 3.875000001229034208 ) ) ;
#2715 = CARTESIAN_POINT ( 'NONE',  ( 3.000000000000004441, 2.000000000000000000, 8.000000000000000000 ) ) ;
#2716 = CARTESIAN_POINT ( 'NONE',  ( 18.35873618070580093, 66.24461453698026503, 0.6666666666666665186 ) ) ;
#2717 = AXIS2_PLACEMENT_3D ( 'NONE', #11906, #9944, #12824 ) ;
#2718 = LINE ( 'NONE', #6564, #9099 ) ;
#2719 = EDGE_CURVE ( 'NONE', #6066, #4728, #2160, .T. ) ;
#2720 = CARTESIAN_POINT ( 'NONE',  ( 3.678215178125014972, 90.00000000000000000, 4.732812500921776078 ) ) ;
#2721 = CARTESIAN_POINT ( 'NONE',  ( 3.556430356250014579, 108.1539533981018053, 4.821875000614516793 ) ) ;
#2722 = ORIENTED_EDGE ( 'NONE', *, *, #9570, .F. ) ;
#2723 = CARTESIAN_POINT ( 'NONE',  ( 3.800000000000015365, 108.0133283987163111, 3.162500000000000533 ) ) ;
#2724 = DIRECTION ( 'NONE',  ( 0.000000000000000000, 0.000000000000000000, 1.000000000000000000 ) ) ;
#2725 = ORIENTED_EDGE ( 'NONE', *, *, #9994, .F. ) ;
#2726 = PRODUCT ( 'socket button head screw_iso_ISO 7380 - M3 x 6 - 6N', 'socket button head screw_iso_ISO 7380 - M3 x 6 - 6N', '', ( #8245 ) ) ;
#2727 = AXIS2_PLACEMENT_3D ( 'NONE', #10655, #10784, #9801 ) ;
#2728 = CARTESIAN_POINT ( 'NONE',  ( 35.00000000000000000, 90.00000000000000000, 4.000000000000000000 ) ) ;
#2729 = LINE ( 'NONE', #2470, #11141 ) ;
#2730 = DIRECTION ( 'NONE',  ( -1.000000000000000000, -0.000000000000000000, -0.000000000000000000 ) ) ;
#2731 = ADVANCED_FACE ( 'NONE', ( #4005 ), #5036, .F. ) ;
#2732 = CARTESIAN_POINT ( 'NONE',  ( 3.556430356250015024, 90.00000000000000000, 3.453125000614517770 ) ) ;
#2733 = EDGE_CURVE ( 'NONE', #5916, #10118, #4195, .T. ) ;
#2734 = CIRCLE ( 'NONE', #2935, 1.000000000000000000 ) ;
#2736 = CIRCLE ( 'NONE', #172, 1.499999999999999778 ) ;
#2735 = PLANE ( 'NONE',  #205 ) ;
#2737 = VERTEX_POINT ( 'NONE', #11113 ) ;
#2738 = DIRECTION ( 'NONE',  ( -1.000000000000000000, 0.000000000000000000, 0.000000000000000000 ) ) ;
#2739 = ORIENTED_EDGE ( 'NONE', *, *, #10530, .T. ) ;
#2740 = FACE_OUTER_BOUND ( 'NONE', #11021, .T. ) ;
#2741 = CARTESIAN_POINT ( 'NONE',  ( 3.000000000000004441, 30.00000000000000000, -8.000000000000000000 ) ) ;
#2742 = AXIS2_PLACEMENT_3D ( 'NONE', #5574, #12709, #9691 ) ;
#2743 = CARTESIAN_POINT ( 'NONE',  ( 35.75000000000000711, 92.49999999999998579, -3.000000000000000000 ) ) ;
#2744 = DIRECTION ( 'NONE',  ( -0.000000000000000000, -0.000000000000000000, -1.000000000000000000 ) ) ;
#2745 = DIRECTION ( 'NONE',  ( -0.000000000000000000, -0.000000000000000000, 1.000000000000000000 ) ) ;
#2746 = CARTESIAN_POINT ( 'NONE',  ( 34.50001850811341342, 118.9978265420697170, -1.000000000000000000 ) ) ;
#2747 = ORIENTED_EDGE ( 'NONE', *, *, #12032, .F. ) ;
#2748 = DIRECTION ( 'NONE',  ( 1.000000000000000000, 0.000000000000000000, 0.000000000000000000 ) ) ;
#2749 = CARTESIAN_POINT ( 'NONE',  ( 45.00000000000000000, 0.000000000000000000, -5.750000000000000000 ) ) ;
#2750 = ORIENTED_EDGE ( 'NONE', *, *, #11121, .F. ) ;
#2751 = DIRECTION ( 'NONE',  ( 1.000000000000000000, 0.000000000000000000, 0.000000000000000000 ) ) ;
#2752 = ORIENTED_EDGE ( 'NONE', *, *, #2404, .F. ) ;
#2753 = AXIS2_PLACEMENT_3D ( 'NONE', #7733, #8779, #10616 ) ;
#2754 = CARTESIAN_POINT ( 'NONE',  ( 17.66025403784438197, 77.14656965084323303, -1.000000000000000000 ) ) ;
#2755 = ORIENTED_EDGE ( 'NONE', *, *, #4012, .F. ) ;
#2756 = ADVANCED_FACE ( 'NONE', ( #6140, #10204 ), #5097, .F. ) ;
#2757 = CARTESIAN_POINT ( 'NONE',  ( 9.934812860078272578, 71.14691728539177973, 3.000000000000000444 ) ) ;
#2758 = LINE ( 'NONE', #10724, #11241 ) ;
#2759 = ORIENTED_EDGE ( 'NONE', *, *, #10639, .T. ) ;
#2760 = AXIS2_PLACEMENT_3D ( 'NONE', #444, #11769, #1893 ) ;
#2761 = DIRECTION ( 'NONE',  ( 1.000000000000000000, 0.000000000000000000, -0.000000000000000000 ) ) ;
#2762 = VERTEX_POINT ( 'NONE', #9091 ) ;
#2763 = APPLICATION_CONTEXT ( 'automotive_design' ) ;
#2764 = CARTESIAN_POINT ( 'NONE',  ( 4.763019983628629994, -4.349268977144817860, -0.8000000000000000444 ) ) ;
#2765 = EDGE_LOOP ( 'NONE', ( #11305, #12086, #8046, #11032 ) ) ;
#2766 = ADVANCED_FACE ( 'NONE', ( #9221 ), #3016, .T. ) ;
#2767 = CARTESIAN_POINT ( 'NONE',  ( 35.00000000000000000, 126.3079067962035822, 4.690625000614518036 ) ) ;
#2768 = ORIENTED_EDGE ( 'NONE', *, *, #12870, .T. ) ;
#2769 = ADVANCED_FACE ( 'NONE', ( #1881 ), #9000, .F. ) ;
#2770 = CARTESIAN_POINT ( 'NONE',  ( 45.00000000000000000, 0.000000000000000000, -7.349999999999996980 ) ) ;
#2771 = LINE ( 'NONE', #6744, #11214 ) ;
#2772 = EDGE_CURVE ( 'NONE', #8971, #3649, #7767, .T. ) ;
#2773 = CIRCLE ( 'NONE', #7992, 28.99999999999999289 ) ;
#2774 = CARTESIAN_POINT ( 'NONE',  ( 66.19999999999997442, 108.0133283987163253, 4.475000001229034297 ) ) ;
#2775 = DIRECTION ( 'NONE',  ( 0.000000000000000000, -1.000000000000000000, 0.000000000000000000 ) ) ;
#2776 = CARTESIAN_POINT ( 'NONE',  ( 64.31840955652157277, 100.6710290542226574, 3.000000000000000000 ) ) ;
#2777 = DIRECTION ( 'NONE',  ( 0.000000000000000000, -0.000000000000000000, 1.000000000000000000 ) ) ;
#2778 = DIRECTION ( 'NONE',  ( -1.000000000000000000, -0.000000000000000000, -0.000000000000000000 ) ) ;
#2779 = CIRCLE ( 'NONE', #8003, 3.350000000000003642 ) ;
#2780 = CARTESIAN_POINT ( 'NONE',  ( 35.00000000000000000, 90.00000000000000000, 5.000000000000000000 ) ) ;
#2781 = EDGE_CURVE ( 'NONE', #10632, #307, #24, .T. ) ;
#2782 = DIRECTION ( 'NONE',  ( 1.000000000000000000, 0.000000000000000000, 0.000000000000000000 ) ) ;
#2783 = CARTESIAN_POINT ( 'NONE',  ( 66.44356964374999563, 71.84604660189820891, 3.696875000614517237 ) ) ;
#2784 = ORIENTED_EDGE ( 'NONE', *, *, #2957, .T. ) ;
#2785 = CARTESIAN_POINT ( 'NONE',  ( 35.00000000000000000, 126.0266567974326222, 4.887500000000001066 ) ) ;
#2786 = CARTESIAN_POINT ( 'NONE',  ( 1.269999999999999796, 0.000000000000000000, 2.849999999999999645 ) ) ;
#2787 = ORIENTED_EDGE ( 'NONE', *, *, #1489, .T. ) ;
#2788 =( NAMED_UNIT ( * ) SI_UNIT ( $, .STERADIAN. ) SOLID_ANGLE_UNIT ( ) );
#2789 =( GEOMETRIC_REPRESENTATION_CONTEXT ( 3 ) GLOBAL_UNCERTAINTY_ASSIGNED_CONTEXT ( ( #1643 ) ) GLOBAL_UNIT_ASSIGNED_CONTEXT ( ( #413, #2467, #6441 ) ) REPRESENTATION_CONTEXT ( 'NONE', 'WORKASPACE' ) );
#2790 = CARTESIAN_POINT ( 'NONE',  ( 35.00000000000000000, 90.00000000000000000, 6.000000000000000000 ) ) ;
#2791 = DIRECTION ( 'NONE',  ( -1.000000000000000000, 0.000000000000000000, 0.000000000000000000 ) ) ;
#2792 = DIRECTION ( 'NONE',  ( 0.000000000000000000, 0.000000000000000000, -1.000000000000000000 ) ) ;
#2793 = CARTESIAN_POINT ( 'NONE',  ( 19.27821517812500574, 117.2309300971526937, 2.928125000614517415 ) ) ;
#2794 = EDGE_CURVE ( 'NONE', #3842, #4251, #11757, .T. ) ;
#2795 = CARTESIAN_POINT ( 'NONE',  ( 3.556430356250015024, 90.00000000000000000, 4.859375000614517326 ) ) ;
#2796 = CARTESIAN_POINT ( 'NONE',  ( 48.49999999999995737, 94.00000000000000000, -10.00000000000000000 ) ) ;
#2797 = ORIENTED_EDGE ( 'NONE', *, *, #4345, .F. ) ;
#2798 = LINE ( 'NONE', #4037, #3708 ) ;
#2799 = ORIENTED_EDGE ( 'NONE', *, *, #1271, .T. ) ;
#2800 = CIRCLE ( 'NONE', #8025, 32.70000000000000995 ) ;
#2801 = CARTESIAN_POINT ( 'NONE',  ( 7.500000000000000000, 27.00000000000000000, 0.000000000000000000 ) ) ;
#2802 = EDGE_CURVE ( 'NONE', #4594, #11781, #10838, .T. ) ;
#2803 = EDGE_CURVE ( 'NONE', #698, #4148, #11946, .T. ) ;
#2804 = AXIS2_PLACEMENT_3D ( 'NONE', #2300, #2234, #11110 ) ;
#2805 = DIRECTION ( 'NONE',  ( 1.000000000000000000, -0.000000000000000000, 0.000000000000000000 ) ) ;
#2806 = CARTESIAN_POINT ( 'NONE',  ( 3.678215178125014972, 90.00000000000000000, 4.929687500307258219 ) ) ;
#2807 = FACE_OUTER_BOUND ( 'NONE', #33, .T. ) ;
#2808 = CARTESIAN_POINT ( 'NONE',  ( 35.00000000000000000, 90.00000000000000000, 6.000000000000000000 ) ) ;
#2809 = ORIENTED_EDGE ( 'NONE', *, *, #5336, .T. ) ;
#2810 = CIRCLE ( 'NONE', #911, 3.499999999999996003 ) ;
#2811 = DIRECTION ( 'NONE',  ( 0.000000000000000000, 0.000000000000000000, 1.000000000000000000 ) ) ;
#2812 = FACE_OUTER_BOUND ( 'NONE', #12565, .T. ) ;
#2813 = CIRCLE ( 'NONE', #8451, 1.425000000000000044 ) ;
#2814 = EDGE_LOOP ( 'NONE', ( #12536, #11570, #363, #2374, #3035 ) ) ;
#2815 = EDGE_CURVE ( 'NONE', #1351, #3214, #3788, .T. ) ;
#2816 = CARTESIAN_POINT ( 'NONE',  ( 7.500000000000000000, 27.00000000000000000, 0.000000000000000000 ) ) ;
#2817 = VERTEX_POINT ( 'NONE', #9856 ) ;
#2818 = PLANE ( 'NONE',  #6930 ) ;
#2819 = VERTEX_POINT ( 'NONE', #1942 ) ;
#2820 = CARTESIAN_POINT ( 'NONE',  ( 35.00000000000000000, 90.00000000000000000, -3.000000000000000000 ) ) ;
#2821 = CARTESIAN_POINT ( 'NONE',  ( -4.270088556250601699E-16, 30.00000000000000000, 8.000000000000000000 ) ) ;
#2822 = CIRCLE ( 'NONE', #4285, 29.99999999999999645 ) ;
#2823 = CIRCLE ( 'NONE', #726, 30.00000000000000000 ) ;
#2824 = ORIENTED_EDGE ( 'NONE', *, *, #9974, .T. ) ;
#2825 = ORIENTED_EDGE ( 'NONE', *, *, #3804, .F. ) ;
#2826 = EDGE_CURVE ( 'NONE', #5941, #3688, #7832, .T. ) ;
#2827 = CARTESIAN_POINT ( 'NONE',  ( -62.42520044359213927, 28.59980987105325667, 0.9999999999999924505 ) ) ;
#2828 = VERTEX_POINT ( 'NONE', #8029 ) ;
#2829 = VECTOR ( 'NONE', #9037, 1000.000000000000000 ) ;
#2830 = DIRECTION ( 'NONE',  ( 0.000000000000000000, -1.000000000000000000, -0.000000000000000000 ) ) ;
#2831 = ORIENTED_EDGE ( 'NONE', *, *, #11272, .T. ) ;
#2832 = AXIS2_PLACEMENT_3D ( 'NONE', #10199, #173, #1167 ) ;
#2833 = DIRECTION ( 'NONE',  ( -0.000000000000000000, 1.000000000000000000, -0.000000000000000000 ) ) ;
#2834 = CARTESIAN_POINT ( 'NONE',  ( 35.00000000000000000, 90.00000000000000000, 1.000000000000003109 ) ) ;
#2835 = PRESENTATION_STYLE_ASSIGNMENT (( #5832 ) ) ;
#2836 = CARTESIAN_POINT ( 'NONE',  ( 50.60000000000001563, 62.98000740192552627, 3.912500001229034297 ) ) ;
#2837 = EDGE_CURVE ( 'NONE', #7663, #9298, #12615, .T. ) ;
#2838 = CIRCLE ( 'NONE', #2203, 28.99999999999999289 ) ;
#2839 = DIRECTION ( 'NONE',  ( -1.000000000000000000, 0.000000000000000000, 0.000000000000000000 ) ) ;
#2840 = DIRECTION ( 'NONE',  ( -1.000000000000000000, -0.000000000000000000, -0.000000000000000000 ) ) ;
#2841 =( BOUNDED_CURVE ( )  B_SPLINE_CURVE ( 2, ( #527, #6488, #5769, #11657, #12649, #594, #1717 ),
 .UNSPECIFIED., .F., .F. ) 
 B_SPLINE_CURVE_WITH_KNOTS ( ( 3, 2, 2, 3 ),
 ( 0.3999999999999999667, 0.4333333333333333481, 0.4666666666666667296, 0.5000000000000001110 ),
 .UNSPECIFIED. ) 
 CURVE ( )  GEOMETRIC_REPRESENTATION_ITEM ( )  RATIONAL_B_SPLINE_CURVE ( ( 1.000000000000000444, 0.8660254037844385966, 1.000000000000000000, 0.8660254037844387076, 1.000000000000000000, 0.8660254037844382635, 1.000000000000000444 ) ) 
 REPRESENTATION_ITEM ( '' )  );
#2842 = CARTESIAN_POINT ( 'NONE',  ( 0.000000000000000000, 0.000000000000000000, 0.000000000000000000 ) ) ;
#2843 = ADVANCED_FACE ( 'NONE', ( #9796 ), #2992, .T. ) ;
#2844 = DIRECTION ( 'NONE',  ( 0.000000000000000000, 0.000000000000000000, -1.000000000000000000 ) ) ;
#2845 = CARTESIAN_POINT ( 'NONE',  ( 1.040000000000000036, -0.5773502691896253980, 1.000000000000000000 ) ) ;
#2846 = CARTESIAN_POINT ( 'NONE',  ( 66.06384527677998619, 99.56752405903819181, 1.000000000000003109 ) ) ;
#2847 = EDGE_LOOP ( 'NONE', ( #1296, #12159, #9133, #10090 ) ) ;
#2848 = DIRECTION ( 'NONE',  ( 0.000000000000000000, 0.000000000000000000, 1.000000000000000000 ) ) ;
#2849 = CIRCLE ( 'NONE', #10145, 1.500000000000001332 ) ;
#2850 = DIRECTION ( 'NONE',  ( 0.000000000000000000, 0.000000000000000000, 1.000000000000000000 ) ) ;
#2851 = EDGE_LOOP ( 'NONE', ( #11355, #4320, #9624, #10703 ) ) ;
#2852 = AXIS2_PLACEMENT_3D ( 'NONE', #4309, #6196, #9338 ) ;
#2853 = CARTESIAN_POINT ( 'NONE',  ( 50.60000000000001563, 62.98000740192552627, 3.800000000000000266 ) ) ;
#2854 = CARTESIAN_POINT ( 'NONE',  ( 0.000000000000000000, 0.000000000000000000, -0.8000000000000000444 ) ) ;
#2855 = EDGE_LOOP ( 'NONE', ( #10880, #2293, #2137, #9670 ) ) ;
#2856 = EDGE_CURVE ( 'NONE', #10254, #10113, #6847, .T. ) ;
#2857 = DIRECTION ( 'NONE',  ( -0.000000000000000000, -0.5000000000000003331, -0.8660254037844383745 ) ) ;
#2858 = EDGE_CURVE ( 'NONE', #6325, #1821, #8876, .T. ) ;
#2859 = CARTESIAN_POINT ( 'NONE',  ( 1.040000000000000036, 0.000000000000000000, -1.000000000000000000 ) ) ;
#2860=STYLED_ITEM('',(#13009),#3541);
#2861 = LINE ( 'NONE', #5855, #8272 ) ;
#2862 = CARTESIAN_POINT ( 'NONE',  ( 3.556430356250014579, 108.1539533981018053, 2.965625000614517504 ) ) ;
#2863 = CARTESIAN_POINT ( 'NONE',  ( 7.650000000000000355, 1.493456771560197319E-16, -1.219500000000000028 ) ) ;
#2864 = DIRECTION ( 'NONE',  ( -0.000000000000000000, -1.000000000000000000, -0.000000000000000000 ) ) ;
#2865 = ORIENTED_EDGE ( 'NONE', *, *, #1503, .T. ) ;
#2866 = CARTESIAN_POINT ( 'NONE',  ( 2.387319993259524598, -4.036502139894371233, 0.000000000000000000 ) ) ;
#2867 = ORIENTED_EDGE ( 'NONE', *, *, #8911, .F. ) ;
#2868 = CIRCLE ( 'NONE', #6403, 1.500000000000001332 ) ;
#2869 = DIRECTION ( 'NONE',  ( 4.336808689942017243E-16, 0.000000000000000000, -1.000000000000000000 ) ) ;
#2870 = EDGE_CURVE ( 'NONE', #2423, #2817, #6718, .T. ) ;
#2871 = CARTESIAN_POINT ( 'NONE',  ( 11.38811426945699345, 73.16316976839823383, -0.9999999999999970024 ) ) ;
#2872 = DIRECTION ( 'NONE',  ( 0.000000000000000000, 0.000000000000000000, 1.000000000000000000 ) ) ;
#2873 = CARTESIAN_POINT ( 'NONE',  ( 35.00000000000000000, 90.00000000000000000, 8.000000000000000000 ) ) ;
#2874 = LINE ( 'NONE', #9609, #3365 ) ;
#2875 = ORIENTED_EDGE ( 'NONE', *, *, #1710, .F. ) ;
#2876 = DIRECTION ( 'NONE',  ( -0.000000000000000000, 1.000000000000000000, -0.000000000000000000 ) ) ;
#2877 = CARTESIAN_POINT ( 'NONE',  ( 7.573869524628007888, 99.43702109502098097, -1.000000000000000000 ) ) ;
#2878 = VECTOR ( 'NONE', #7793, 1000.000000000000000 ) ;
#2879 = ORIENTED_EDGE ( 'NONE', *, *, #9817, .T. ) ;
#2880 = CYLINDRICAL_SURFACE ( 'NONE', #1582, 1.599999999999992095 ) ;
#2881 = ORIENTED_EDGE ( 'NONE', *, *, #4201, .T. ) ;
#2882 = EDGE_CURVE ( 'NONE', #12839, #3511, #6115, .T. ) ;
#2883 = CYLINDRICAL_SURFACE ( 'NONE', #2131, 3.349999999999995204 ) ;
#2884 = EDGE_LOOP ( 'NONE', ( #11242, #3591, #10722 ) ) ;
#2885 = FACE_OUTER_BOUND ( 'NONE', #8367, .T. ) ;
#2886 = DIRECTION ( 'NONE',  ( 0.000000000000000000, 0.000000000000000000, -1.000000000000000000 ) ) ;
#2887 = CIRCLE ( 'NONE', #7257, 10.00000000000000178 ) ;
#2888 = ORIENTED_EDGE ( 'NONE', *, *, #3152, .F. ) ;
#2889 = LINE ( 'NONE', #6674, #8057 ) ;
#2890 = EDGE_LOOP ( 'NONE', ( #12441, #3402, #12951, #5471 ) ) ;
#2891 = LINE ( 'NONE', #1901, #5631 ) ;
#2892 = ORIENTED_EDGE ( 'NONE', *, *, #8557, .F. ) ;
#2893 = CARTESIAN_POINT ( 'NONE',  ( 66.44356964374999563, 90.00000000000000000, 3.228125000614517237 ) ) ;
#2894 = VECTOR ( 'NONE', #2612, 1000.000000000000000 ) ;
#2895 = EDGE_LOOP ( 'NONE', ( #1089, #6800 ) ) ;
#2896 = VECTOR ( 'NONE', #5363, 1000.000000000000000 ) ;
#2897 = EDGE_CURVE ( 'NONE', #1898, #585, #10897, .T. ) ;
#2898 = CARTESIAN_POINT ( 'NONE',  ( -64.48205080756885366, 31.76313972081441150, 1.836970198721030427E-16 ) ) ;
#2899 = CARTESIAN_POINT ( 'NONE',  ( 35.49999999999994316, 119.9958330439412890, 1.000000000000003109 ) ) ;
#2900 = CARTESIAN_POINT ( 'NONE',  ( 23.09999999999997300, 90.00000000000000000, -10.00000000000000178 ) ) ;
#2901 = CARTESIAN_POINT ( 'NONE',  ( 50.72178482187499071, 117.2309300971526937, 2.853125000614517237 ) ) ;
#2902 = FACE_OUTER_BOUND ( 'NONE', #7339, .T. ) ;
#2903 = VECTOR ( 'NONE', #1229, 1000.000000000000114 ) ;
#2904 = EDGE_LOOP ( 'NONE', ( #7306, #10371, #9401, #8329, #6249 ) ) ;
#2905 = FACE_OUTER_BOUND ( 'NONE', #9710, .T. ) ;
#2906 = DIRECTION ( 'NONE',  ( -1.000000000000000000, 0.000000000000000000, -5.337610695313252124E-17 ) ) ;
#2907 = LINE ( 'NONE', #3954, #7624 ) ;
#2908 = ORIENTED_EDGE ( 'NONE', *, *, #8160, .T. ) ;
#2909 = LINE ( 'NONE', #2846, #8897 ) ;
#2910 = ORIENTED_EDGE ( 'NONE', *, *, #693, .T. ) ;
#2911 = DIRECTION ( 'NONE',  ( 0.000000000000000000, 0.000000000000000000, 1.000000000000000000 ) ) ;
#2912 = CARTESIAN_POINT ( 'NONE',  ( 36.50000000000001421, 67.79999999999999716, 8.000000000000000000 ) ) ;
#2913 = ORIENTED_EDGE ( 'NONE', *, *, #12321, .F. ) ;
#2914 = CARTESIAN_POINT ( 'NONE',  ( 66.44356964374999563, 71.84604660189820891, 4.596875000614517148 ) ) ;
#2915 = DIRECTION ( 'NONE',  ( -0.000000000000000000, 1.000000000000000000, -0.000000000000000000 ) ) ;
#2916 = EDGE_CURVE ( 'NONE', #10444, #3526, #1751, .T. ) ;
#2917 = VECTOR ( 'NONE', #9628, 1000.000000000000000 ) ;
#2918 = DIRECTION ( 'NONE',  ( -0.8660254037844361541, -0.5000000000000042188, 0.000000000000000000 ) ) ;
#2919 = B_SPLINE_CURVE_WITH_KNOTS ( 'NONE', 3,
 ( #354, #5142, #10181, #4365 ),
 .UNSPECIFIED., .F., .F.,
 ( 4, 4 ),
 ( 0.000000000000000000, 0.5999999999999994227 ),
 .UNSPECIFIED. ) ;
#2920 = CYLINDRICAL_SURFACE ( 'NONE', #12831, 1.599999999999993872 ) ;
#2921 = AXIS2_PLACEMENT_3D ( 'NONE', #9697, #11792, #2839 ) ;
#2922 = DIRECTION ( 'NONE',  ( -0.000000000000000000, 1.000000000000000000, -0.000000000000000000 ) ) ;
#2923 = LINE ( 'NONE', #4944, #12758 ) ;
#2924 = CARTESIAN_POINT ( 'NONE',  ( 50.72178482187501203, 62.76906990284730625, 4.109375000614517326 ) ) ;
#2925 = ORIENTED_EDGE ( 'NONE', *, *, #2364, .T. ) ;
#2926 = EDGE_CURVE ( 'NONE', #9339, #1634, #6783, .T. ) ;
#2927 = CIRCLE ( 'NONE', #10231, 6.499999999999999112 ) ;
#2928 = CARTESIAN_POINT ( 'NONE',  ( 62.42406877824604550, 99.43633191144624561, -1.000000000000000222 ) ) ;
#2929 = ORIENTED_EDGE ( 'NONE', *, *, #11621, .T. ) ;
#2930 = EDGE_CURVE ( 'NONE', #6279, #8102, #11826, .T. ) ;
#2931 = LINE ( 'NONE', #7962, #9256 ) ;
#2932 =( REPRESENTATION_RELATIONSHIP ('NONE','NONE', #1997, #11692 ) REPRESENTATION_RELATIONSHIP_WITH_TRANSFORMATION ( #10654 )SHAPE_REPRESENTATION_RELATIONSHIP( ) );
#2933 = DIRECTION ( 'NONE',  ( -0.000000000000000000, -0.000000000000000000, -1.000000000000000000 ) ) ;
#2934 = DIRECTION ( 'NONE',  ( -0.000000000000000000, 0.5000000000000000000, 0.8660254037844385966 ) ) ;
#2936 = FACE_OUTER_BOUND ( 'NONE', #9647, .T. ) ;
#2935 = AXIS2_PLACEMENT_3D ( 'NONE', #6372, #4293, #8475 ) ;
#2937 = EDGE_LOOP ( 'NONE', ( #5814, #4900, #5525, #676 ) ) ;
#2938 = DIRECTION ( 'NONE',  ( -1.000000000000000000, -0.000000000000000000, -0.000000000000000000 ) ) ;
#2939 = DIRECTION ( 'NONE',  ( 1.000000000000000000, 0.000000000000000000, -0.000000000000000000 ) ) ;
#2940 = VERTEX_POINT ( 'NONE', #11887 ) ;
#2941 = LINE ( 'NONE', #32, #8499 ) ;
#2942 = EDGE_LOOP ( 'NONE', ( #9453, #368 ) ) ;
#2943 = EDGE_CURVE ( 'NONE', #2819, #11286, #4048, .T. ) ;
#2944 = ORIENTED_EDGE ( 'NONE', *, *, #9951, .T. ) ;
#2945 = DIRECTION ( 'NONE',  ( -0.000000000000000000, -0.000000000000000000, -1.000000000000000000 ) ) ;
#2946 = VECTOR ( 'NONE', #6500, 1000.000000000000000 ) ;
#2947 = LINE ( 'NONE', #12819, #7492 ) ;
#2948 = ORIENTED_EDGE ( 'NONE', *, *, #9418, .F. ) ;
#2949 = ORIENTED_EDGE ( 'NONE', *, *, #10700, .T. ) ;
#2950 = DIRECTION ( 'NONE',  ( -0.000000000000000000, -0.000000000000000000, -1.000000000000000000 ) ) ;
#2951 = ORIENTED_EDGE ( 'NONE', *, *, #12396, .T. ) ;
#2952 = FACE_BOUND ( 'NONE', #9002, .T. ) ;
#2953 = ORIENTED_EDGE ( 'NONE', *, *, #11170, .T. ) ;
#2954 = VECTOR ( 'NONE', #6822, 1000.000000000000000 ) ;
#2955 = CARTESIAN_POINT ( 'NONE',  ( 66.44356964374999563, 90.00000000000000000, 4.578125000614516438 ) ) ;
#2956 = ORIENTED_EDGE ( 'NONE', *, *, #9180, .F. ) ;
#2957 = EDGE_CURVE ( 'NONE', #1779, #7089, #3911, .T. ) ;
#2958 = CARTESIAN_POINT ( 'NONE',  ( 3.800000000000015365, 90.00000000000000000, 4.662500001229034297 ) ) ;
#2959 = CARTESIAN_POINT ( 'NONE',  ( 66.44356964374998142, 108.1539533981018053, 3.715625000614517948 ) ) ;
#2960 = PLANE ( 'NONE',  #4438 ) ;
#2961 = CARTESIAN_POINT ( 'NONE',  ( 50.72178482187499071, 117.2309300971526937, 3.303125000614517415 ) ) ;
#2962 = AXIS2_PLACEMENT_3D ( 'NONE', #4327, #6341, #119 ) ;
#2963 = LINE ( 'NONE', #3695, #8345 ) ;
#2964 = EDGE_CURVE ( 'NONE', #8808, #5624, #220, .T. ) ;
#2966 = ADVANCED_FACE ( 'NONE', ( #11157 ), #3262, .F. ) ;
#2965 = ORIENTED_EDGE ( 'NONE', *, *, #12332, .F. ) ;
#2967 = CARTESIAN_POINT ( 'NONE',  ( 64.26751784650379307, 100.8093265756609185, 3.000000000000000000 ) ) ;
#2968 = LINE ( 'NONE', #1984, #11678 ) ;
#2969 = LINE ( 'NONE', #5778, #3868 ) ;
#2970 = VERTEX_POINT ( 'NONE', #1145 ) ;
#2971 = CARTESIAN_POINT ( 'NONE',  ( 35.00000000000000000, 90.00000000000000000, -3.000000000000000888 ) ) ;
#2972 = EDGE_LOOP ( 'NONE', ( #6291, #3797, #12728, #2237, #1074, #5573, #781, #10453, #11927, #9042, #4114, #888, #12061, #3449, #5344, #4146, #849, #2787, #1828, #11545 ) ) ;
#2973 = CARTESIAN_POINT ( 'NONE',  ( 4.336808689942017736E-16, 0.000000000000000000, 0.000000000000000000 ) ) ;
#2974 = CARTESIAN_POINT ( 'NONE',  ( 66.44356964374999563, 90.00000000000000000, 4.634375000614516793 ) ) ;
#2975 = ORIENTED_EDGE ( 'NONE', *, *, #8127, .T. ) ;
#2976 = CARTESIAN_POINT ( 'NONE',  ( 19.27821517812503060, 62.76906990284727783, 4.484375000614516438 ) ) ;
#2977 = DIRECTION ( 'NONE',  ( -1.000000000000000000, 0.000000000000000000, -0.000000000000000000 ) ) ;
#2978 = CIRCLE ( 'NONE', #11953, 1.500000000000001332 ) ;
#2979 = DIRECTION ( 'NONE',  ( -0.000000000000000000, -0.000000000000000000, 1.000000000000000000 ) ) ;
#2980 = CARTESIAN_POINT ( 'NONE',  ( 45.00000000000000000, 2.000000000000000000, 5.750000000000000888 ) ) ;
#2981 = CARTESIAN_POINT ( 'NONE',  ( -4.270088556250601699E-16, 30.00000000000000000, 8.000000000000000000 ) ) ;
#2982 = EDGE_CURVE ( 'NONE', #10475, #2423, #5715, .T. ) ;
#2983 = CARTESIAN_POINT ( 'NONE',  ( 4.338286831716297698, 0.4117131682837005258, -0.8000000000000000444 ) ) ;
#2984 = CARTESIAN_POINT ( 'NONE',  ( -1.000000000000000000, -5.473461295629626022, -0.8000000000000000444 ) ) ;
#2985 = EDGE_LOOP ( 'NONE', ( #9465, #9544, #12255, #9850 ) ) ;
#2986 = AXIS2_PLACEMENT_3D ( 'NONE', #11038, #2026, #2091 ) ;
#2987 =( BOUNDED_CURVE ( )  B_SPLINE_CURVE ( 2, ( #7499, #4428, #415, #10743, #8784, #7367, #3453 ),
 .UNSPECIFIED., .F., .F. ) 
 B_SPLINE_CURVE_WITH_KNOTS ( ( 3, 2, 2, 3 ),
 ( 0.1000000000000001860, 0.1333333333333334425, 0.1666666666666666852, 0.2000000000000000111 ),
 .UNSPECIFIED. ) 
 CURVE ( )  GEOMETRIC_REPRESENTATION_ITEM ( )  RATIONAL_B_SPLINE_CURVE ( ( 0.9999999999999992228, 0.8660254037844394848, 1.000000000000000000, 0.8660254037844387076, 1.000000000000000000, 0.8660254037844388186, 0.9999999999999998890 ) ) 
 REPRESENTATION_ITEM ( '' )  );
#2988 = CARTESIAN_POINT ( 'NONE',  ( 5.000000000000004441, 0.000000000000000000, 10.00000000000000000 ) ) ;
#2989 = VERTEX_POINT ( 'NONE', #10246 ) ;
#2990 = DIRECTION ( 'NONE',  ( 1.000000000000000000, 0.000000000000000000, 0.000000000000000000 ) ) ;
#2991 = FACE_OUTER_BOUND ( 'NONE', #8772, .T. ) ;
#2993 = EDGE_CURVE ( 'NONE', #2819, #6338, #2340, .T. ) ;
#2992 = CYLINDRICAL_SURFACE ( 'NONE', #10087, 4.000000000000000000 ) ;
#2994 = CARTESIAN_POINT ( 'NONE',  ( -61.13397459621555186, 31.96410161513774284, 0.000000000000000000 ) ) ;
#2995 = MECHANICAL_DESIGN_GEOMETRIC_PRESENTATION_REPRESENTATION (  '', ( #9040 ), #10302 ) ;
#2996 = ORIENTED_EDGE ( 'NONE', *, *, #12229, .F. ) ;
#2997 = FACE_OUTER_BOUND ( 'NONE', #12705, .T. ) ;
#2998 = ADVANCED_FACE ( 'NONE', ( #4238 ), #12013, .T. ) ;
#2999 = CARTESIAN_POINT ( 'NONE',  ( 3.800000000000015365, 90.00000000000000000, 4.212500001229034119 ) ) ;
#3000 = ORIENTED_EDGE ( 'NONE', *, *, #5978, .F. ) ;
#3001 = SURFACE_STYLE_USAGE ( .BOTH. , #1024 ) ;
#3002 = VECTOR ( 'NONE', #951, 1000.000000000000000 ) ;
#3003 = ORIENTED_EDGE ( 'NONE', *, *, #6590, .F. ) ;
#3004 = DIRECTION ( 'NONE',  ( -0.000000000000000000, -0.000000000000000000, -1.000000000000000000 ) ) ;
#3005 = ORIENTED_EDGE ( 'NONE', *, *, #8313, .F. ) ;
#3006 = FACE_OUTER_BOUND ( 'NONE', #11503, .T. ) ;
#3007 = CARTESIAN_POINT ( 'NONE',  ( 64.31840935109022439, 100.6710296186405742, 2.661976390793298286 ) ) ;
#3008 = ORIENTED_EDGE ( 'NONE', *, *, #5699, .T. ) ;
#3009 = VECTOR ( 'NONE', #4890, 1000.000000000000227 ) ;
#3010 = EDGE_CURVE ( 'NONE', #7510, #3209, #7171, .T. ) ;
#3011 = ORIENTED_EDGE ( 'NONE', *, *, #3949, .T. ) ;
#3012 = LINE ( 'NONE', #4255, #9921 ) ;
#3013 = ORIENTED_EDGE ( 'NONE', *, *, #10275, .F. ) ;
#3014 = CARTESIAN_POINT ( 'NONE',  ( 7.500000000000000000, 30.00000000000000000, 1.499999999999999556 ) ) ;
#3015 = VERTEX_POINT ( 'NONE', #154 ) ;
#3016 = PLANE ( 'NONE',  #263 ) ;
#3017 = VERTEX_POINT ( 'NONE', #11224 ) ;
#3018 = CARTESIAN_POINT ( 'NONE',  ( 45.00000000000000000, 0.000000000000000000, -7.250000000000000888 ) ) ;
#3019 = VECTOR ( 'NONE', #4351, 1000.000000000000000 ) ;
#3020 = CARTESIAN_POINT ( 'NONE',  ( 3.556430356250014135, 90.74660626562589982, 3.001582761613071693 ) ) ;
#3021 = CIRCLE ( 'NONE', #5091, 1.500000000000001332 ) ;
#3022 = FACE_BOUND ( 'NONE', #6719, .T. ) ;
#3023 = CARTESIAN_POINT ( 'NONE',  ( 35.00000000000000000, 126.0266567974326222, 3.200000001229034385 ) ) ;
#3024 =( LENGTH_UNIT ( ) NAMED_UNIT ( * ) SI_UNIT ( .MILLI., .METRE. ) );
#3025 = CARTESIAN_POINT ( 'NONE',  ( 7.264852530253062213, 98.48596457872582732, -1.000000000000000000 ) ) ;
#3026 = EDGE_CURVE ( 'NONE', #4743, #12641, #3062, .T. ) ;
#3027 = ORIENTED_EDGE ( 'NONE', *, *, #1765, .F. ) ;
#3028 = CARTESIAN_POINT ( 'NONE',  ( 19.40000000000000924, 117.0199925980744666, 3.575000000000000178 ) ) ;
#3029 = CIRCLE ( 'NONE', #921, 1.500000000000001332 ) ;
#3030 = DIRECTION ( 'NONE',  ( -1.000000000000000000, 0.000000000000000000, 0.000000000000000000 ) ) ;
#3031 = CARTESIAN_POINT ( 'NONE',  ( 53.14830700235364702, 115.4796592025445392, 2.999999999999999556 ) ) ;
#3032 = ORIENTED_EDGE ( 'NONE', *, *, #10147, .F. ) ;
#3033 = AXIS2_PLACEMENT_3D ( 'NONE', #7800, #3952, #9766 ) ;
#3034 = CARTESIAN_POINT ( 'NONE',  ( 64.54729015011659499, 100.7543347877113717, 2.821351390178781227 ) ) ;
#3035 = ORIENTED_EDGE ( 'NONE', *, *, #2445, .F. ) ;
#3036 = LINE ( 'NONE', #9043, #11717 ) ;
#3037 = UNCERTAINTY_MEASURE_WITH_UNIT (LENGTH_MEASURE( 1.000000000000000082E-05 ), #7177, 'distance_accuracy_value', 'NONE');
#3038 = CARTESIAN_POINT ( 'NONE',  ( 66.44356964374998142, 108.1539533981018053, 4.615625000614516971 ) ) ;
#3040 = EDGE_CURVE ( 'NONE', #4006, #3240, #743, .T. ) ;
#3039 = VERTEX_POINT ( 'NONE', #7043 ) ;
#3041 = ADVANCED_FACE ( 'NONE', ( #1215 ), #8221, .F. ) ;
#3042 = CARTESIAN_POINT ( 'NONE',  ( 50.72178482187499071, 117.2309300971526937, 4.709375000614516971 ) ) ;
#3043 = CARTESIAN_POINT ( 'NONE',  ( 0.000000000000000000, 0.000000000000000000, 0.000000000000000000 ) ) ;
#3044 = VECTOR ( 'NONE', #3393, 1000.000000000000000 ) ;
#3045 = DIRECTION ( 'NONE',  ( 0.000000000000000000, 0.000000000000000000, 1.000000000000000000 ) ) ;
#3046 = CIRCLE ( 'NONE', #935, 1.599999999999990319 ) ;
#3047 = CYLINDRICAL_SURFACE ( 'NONE', #284, 3.499999999999996003 ) ;
#3048 = EDGE_CURVE ( 'NONE', #1413, #39, #9521, .T. ) ;
#3049 = FACE_BOUND ( 'NONE', #4853, .T. ) ;
#3050 = AXIS2_PLACEMENT_3D ( 'NONE', #12331, #8279, #1401 ) ;
#3051 = CARTESIAN_POINT ( 'NONE',  ( 9.999999999999994671, 76.58915998087155685, 2.500000000000000444 ) ) ;
#3052=STYLED_ITEM('',(#12988),#3308);
#3053 = DIRECTION ( 'NONE',  ( 0.000000000000000000, 0.000000000000000000, 1.000000000000000000 ) ) ;
#3054 = LINE ( 'NONE', #7036, #8289 ) ;
#3055 = ORIENTED_EDGE ( 'NONE', *, *, #8182, .T. ) ;
#3056 = EDGE_CURVE ( 'NONE', #870, #6548, #12862, .T. ) ;
#3057 = DIRECTION ( 'NONE',  ( 1.000000000000000000, 0.000000000000000000, 0.000000000000000000 ) ) ;
#3058 = ORIENTED_EDGE ( 'NONE', *, *, #10619, .F. ) ;
#3059 = EDGE_CURVE ( 'NONE', #8545, #12789, #3193, .T. ) ;
#3060 = CIRCLE ( 'NONE', #5972, 3.350000000000003642 ) ;
#3061 = DIRECTION ( 'NONE',  ( -0.000000000000000000, -0.000000000000000000, -1.000000000000000000 ) ) ;
#3062 = LINE ( 'NONE', #5140, #11403 ) ;
#3063 = CARTESIAN_POINT ( 'NONE',  ( 25.00000000000000355, 0.000000000000000000, -5.750000000000000000 ) ) ;
#3064 = EDGE_LOOP ( 'NONE', ( #2298, #2564 ) ) ;
#3065 = DIRECTION ( 'NONE',  ( -0.9510565162951543083, 0.3090169943749451198, 0.000000000000000000 ) ) ;
#3066 = CARTESIAN_POINT ( 'NONE',  ( 50.60000000000001563, 62.98000740192552627, 3.800000000000000266 ) ) ;
#3067 = ORIENTED_EDGE ( 'NONE', *, *, #9983, .F. ) ;
#3068 =( BOUNDED_CURVE ( )  B_SPLINE_CURVE ( 2, ( #7082, #12055, #12316, #6232, #3103, #3169, #12254 ),
 .UNSPECIFIED., .F., .T. ) 
 B_SPLINE_CURVE_WITH_KNOTS ( ( 3, 2, 2, 3 ),
 ( 0.5000000000000001110, 0.5333333333333334370, 0.5666666666666666519, 0.5999999999999999778 ),
 .UNSPECIFIED. ) 
 CURVE ( )  GEOMETRIC_REPRESENTATION_ITEM ( )  RATIONAL_B_SPLINE_CURVE ( ( 0.9999999999999995559, 0.8660254037844391517, 1.000000000000000000, 0.8660254037844387076, 1.000000000000000000, 0.8660254037844387076, 1.000000000000000000 ) ) 
 REPRESENTATION_ITEM ( '' )  );
#3069 =( LENGTH_UNIT ( ) NAMED_UNIT ( * ) SI_UNIT ( .MILLI., .METRE. ) );
#3070 = PLANE ( 'NONE',  #9530 ) ;
#3071 = ORIENTED_EDGE ( 'NONE', *, *, #791, .F. ) ;
#3072 = AXIS2_PLACEMENT_3D ( 'NONE', #2912, #8791, #2850 ) ;
#3073 = ADVANCED_FACE ( 'NONE', ( #286 ), #1344, .T. ) ;
#3074 = CARTESIAN_POINT ( 'NONE',  ( -61.00000000000000711, 31.73205080756887142, 3.000000000000000000 ) ) ;
#3075 = ORIENTED_EDGE ( 'NONE', *, *, #9857, .T. ) ;
#3076 = PLANE ( 'NONE',  #10502 ) ;
#3077 = CARTESIAN_POINT ( 'NONE',  ( 38.50000000000000711, 90.00000000000000000, -8.000000000000000000 ) ) ;
#3078 = ADVANCED_FACE ( 'NONE', ( #3127 ), #6749, .T. ) ;
#3079 = VERTEX_POINT ( 'NONE', #1788 ) ;
#3080 = ORIENTED_EDGE ( 'NONE', *, *, #2269, .T. ) ;
#3081 = AXIS2_PLACEMENT_3D ( 'NONE', #11941, #5917, #3912 ) ;
#3082 = CARTESIAN_POINT ( 'NONE',  ( 35.00000000000000000, 90.00000000000000000, 5.000000000000000000 ) ) ;
#3083 = ORIENTED_EDGE ( 'NONE', *, *, #4687, .F. ) ;
#3084 = APPLICATION_PROTOCOL_DEFINITION ( 'draft international standard', 'automotive_design', 1998, #232 ) ;
#3085 = CARTESIAN_POINT ( 'NONE',  ( 66.44356964374999563, 71.84604660189820891, 3.190625000614517592 ) ) ;
#3086 = ORIENTED_EDGE ( 'NONE', *, *, #895, .T. ) ;
#3087 = DIRECTION ( 'NONE',  ( 0.000000000000000000, 0.000000000000000000, 1.000000000000000000 ) ) ;
#3088 = ORIENTED_EDGE ( 'NONE', *, *, #9280, .F. ) ;
#3089 = DIRECTION ( 'NONE',  ( 0.000000000000000000, 0.000000000000000000, 1.000000000000000000 ) ) ;
#3090 = CARTESIAN_POINT ( 'NONE',  ( 3.556430356250028790, 71.84604660189818048, 3.490625000614516971 ) ) ;
#3091 = EDGE_CURVE ( 'NONE', #4148, #4871, #9456, .T. ) ;
#3092 = AXIS2_PLACEMENT_3D ( 'NONE', #11807, #7750, #745 ) ;
#3093 = LINE ( 'NONE', #5103, #1298 ) ;
#3094 = CARTESIAN_POINT ( 'NONE',  ( 31.86464806177570352, 88.44450386581220869, -3.000000000000000888 ) ) ;
#3095 = ADVANCED_FACE ( 'NONE', ( #7433 ), #11550, .F. ) ;
#3096 = CARTESIAN_POINT ( 'NONE',  ( 32.09707732552327286, 88.32801317409231956, -3.800000000000000266 ) ) ;
#3097 = VERTEX_POINT ( 'NONE', #481 ) ;
#3098 = CARTESIAN_POINT ( 'NONE',  ( 19.40000000000000924, 117.0199925980744666, 4.474999999999999645 ) ) ;
#3099 = CARTESIAN_POINT ( 'NONE',  ( 17.49999999999998579, 90.00000000000002842, -10.00000000000000000 ) ) ;
#3100 = DIRECTION ( 'NONE',  ( 1.000000000000000000, 0.000000000000000000, 0.000000000000000000 ) ) ;
#3101 = VECTOR ( 'NONE', #1575, 1000.000000000000000 ) ;
#3102 = EDGE_LOOP ( 'NONE', ( #385, #5025 ) ) ;
#3103 = CARTESIAN_POINT ( 'NONE',  ( 19.40000000000002700, 62.98000740192551206, 3.725000000000000089 ) ) ;
#3104 = ORIENTED_EDGE ( 'NONE', *, *, #11838, .F. ) ;
#3105 = LINE ( 'NONE', #1923, #3786 ) ;
#3106 = CARTESIAN_POINT ( 'NONE',  ( 50.72178482187499071, 117.2309300971526937, 4.653125000614517504 ) ) ;
#3107 = EDGE_LOOP ( 'NONE', ( #901, #816, #9398, #233 ) ) ;
#3108 = EDGE_CURVE ( 'NONE', #5993, #4459, #10442, .T. ) ;
#3109 = CARTESIAN_POINT ( 'NONE',  ( 3.556430356250015024, 90.00000000000000000, 4.409375000614517148 ) ) ;
#3110 = DIRECTION ( 'NONE',  ( -0.000000000000000000, 1.000000000000000000, -0.000000000000000000 ) ) ;
#3111 = VECTOR ( 'NONE', #4363, 1000.000000000000000 ) ;
#3113 = CIRCLE ( 'NONE', #3943, 1.500000000000001332 ) ;
#3112 = DIRECTION ( 'NONE',  ( 0.1305261922200528224, -0.9914448613738103822, 0.000000000000000000 ) ) ;
#3114 = LINE ( 'NONE', #4223, #293 ) ;
#3115 = FACE_OUTER_BOUND ( 'NONE', #819, .T. ) ;
#3116 = CARTESIAN_POINT ( 'NONE',  ( 45.00000000000000000, -5.000000000000000000, 7.250000000000001776 ) ) ;
#3117 = AXIS2_PLACEMENT_3D ( 'NONE', #3412, #3288, #2431 ) ;
#3118 = LINE ( 'NONE', #10171, #7110 ) ;
#3119 = CARTESIAN_POINT ( 'NONE',  ( 19.27821517812503060, 62.76906990284727783, 3.584375000614516971 ) ) ;
#3120 = ORIENTED_EDGE ( 'NONE', *, *, #4526, .T. ) ;
#3121 = LINE ( 'NONE', #1075, #7040 ) ;
#3122 = ORIENTED_EDGE ( 'NONE', *, *, #5106, .T. ) ;
#3123 = SURFACE_STYLE_FILL_AREA ( #4362 ) ;
#3124 = CIRCLE ( 'NONE', #8956, 1.499999999999999778 ) ;
#3125 = AXIS2_PLACEMENT_3D ( 'NONE', #8782, #9827, #11661 ) ;
#3126 = DIRECTION ( 'NONE',  ( 0.4999999999999995559, -0.8660254037844389297, 0.000000000000000000 ) ) ;
#3127 = FACE_OUTER_BOUND ( 'NONE', #4038, .T. ) ;
#3128 = EDGE_CURVE ( 'NONE', #7460, #1779, #2987, .T. ) ;
#3129 = FACE_OUTER_BOUND ( 'NONE', #9879, .T. ) ;
#3130 = EDGE_CURVE ( 'NONE', #5549, #4991, #4493, .T. ) ;
#3131 = ORIENTED_EDGE ( 'NONE', *, *, #9805, .F. ) ;
#3132 = DIRECTION ( 'NONE',  ( 0.000000000000000000, 0.000000000000000000, -1.000000000000000000 ) ) ;
#3133 = FACE_OUTER_BOUND ( 'NONE', #1801, .T. ) ;
#3134 = ORIENTED_EDGE ( 'NONE', *, *, #4074, .T. ) ;
#3135 = VECTOR ( 'NONE', #4800, 1000.000000000000000 ) ;
#3136 = SURFACE_STYLE_FILL_AREA ( #12943 ) ;
#3137 = SURFACE_SIDE_STYLE ('',( #8101 ) ) ;
#3138 = ORIENTED_EDGE ( 'NONE', *, *, #9857, .F. ) ;
#3139 = DIRECTION ( 'NONE',  ( 0.000000000000000000, 0.000000000000000000, 1.000000000000000000 ) ) ;
#3140 = EDGE_LOOP ( 'NONE', ( #3540, #7051, #10160 ) ) ;
#3141 = CARTESIAN_POINT ( 'NONE',  ( 19.40000000000000924, 117.0199925980744666, 4.587500001229034119 ) ) ;
#3142 = DIRECTION ( 'NONE',  ( 0.000000000000000000, 0.000000000000000000, 1.000000000000000000 ) ) ;
#3143 = VERTEX_POINT ( 'NONE', #3820 ) ;
#3144 = VECTOR ( 'NONE', #12283, 1000.000000000000000 ) ;
#3145 = ORIENTED_EDGE ( 'NONE', *, *, #2299, .F. ) ;
#3146 = FACE_OUTER_BOUND ( 'NONE', #8120, .T. ) ;
#3147 = ORIENTED_EDGE ( 'NONE', *, *, #12775, .F. ) ;
#3148 = DIRECTION ( 'NONE',  ( 0.1884548733085491812, 0.000000000000000000, 0.9820818503191365290 ) ) ;
#3149 = CARTESIAN_POINT ( 'NONE',  ( 3.800000000000015365, 90.00000000000000000, 4.662500001229034297 ) ) ;
#3150 = VERTEX_POINT ( 'NONE', #5396 ) ;
#3151 = CARTESIAN_POINT ( 'NONE',  ( 19.40000000000002700, 62.98000740192551206, 3.387500001229033941 ) ) ;
#3152 = EDGE_CURVE ( 'NONE', #8914, #6886, #2403, .T. ) ;
#3153 = DIRECTION ( 'NONE',  ( 0.000000000000000000, 0.000000000000000000, 1.000000000000000000 ) ) ;
#3154 = EDGE_LOOP ( 'NONE', ( #8578, #623, #2679, #7603, #5681 ) ) ;
#3155 = VECTOR ( 'NONE', #4880, 1000.000000000000000 ) ;
#3156 = DIRECTION ( 'NONE',  ( -1.000000000000000000, 0.000000000000000000, -5.337610695313252124E-17 ) ) ;
#3157 = CARTESIAN_POINT ( 'NONE',  ( 19.27821517812503060, 62.76906990284727783, 3.978125000614516793 ) ) ;
#3158 = CARTESIAN_POINT ( 'NONE',  ( 19.40000000000000924, 117.0199925980744666, 4.924999999999999822 ) ) ;
#3159 = CARTESIAN_POINT ( 'NONE',  ( 50.60000000000001563, 62.98000740192552627, 3.462500001229034563 ) ) ;
#3160 =( NAMED_UNIT ( * ) SI_UNIT ( $, .STERADIAN. ) SOLID_ANGLE_UNIT ( ) );
#3161 = FACE_OUTER_BOUND ( 'NONE', #9940, .T. ) ;
#3162 = ORIENTED_EDGE ( 'NONE', *, *, #2094, .T. ) ;
#3163 = VECTOR ( 'NONE', #1387, 1000.000000000000000 ) ;
#3164 = CARTESIAN_POINT ( 'NONE',  ( 50.60000000000001563, 62.98000740192552627, 3.800000000000000266 ) ) ;
#3165 = EDGE_CURVE ( 'NONE', #9939, #11636, #9935, .T. ) ;
#3166 = DIRECTION ( 'NONE',  ( 0.000000000000000000, -1.000000000000000000, 0.000000000000000000 ) ) ;
#3167 = DIRECTION ( 'NONE',  ( 0.000000000000000000, 0.000000000000000000, 1.000000000000000000 ) ) ;
#3168 = VERTEX_POINT ( 'NONE', #793 ) ;
#3169 = CARTESIAN_POINT ( 'NONE',  ( 3.800000000000025580, 71.98667160128366049, 3.687500000000000888 ) ) ;
#3170 = EDGE_CURVE ( 'NONE', #5032, #242, #7642, .T. ) ;
#3171 = ORIENTED_EDGE ( 'NONE', *, *, #4593, .F. ) ;
#3172 = DIRECTION ( 'NONE',  ( 0.000000000000000000, -1.000000000000000000, 0.000000000000000000 ) ) ;
#3173 = CARTESIAN_POINT ( 'NONE',  ( 35.00000000000000000, 126.3079067962035822, 3.340625000614517059 ) ) ;
#3174 = VERTEX_POINT ( 'NONE', #10809 ) ;
#3175 = CARTESIAN_POINT ( 'NONE',  ( 35.00000000000000000, 126.3079067962035822, 2.946875000614516793 ) ) ;
#3176 = AXIS2_PLACEMENT_3D ( 'NONE', #8251, #8122, #12173 ) ;
#3177 = DIRECTION ( 'NONE',  ( 1.000000000000000000, 0.000000000000000000, 0.000000000000000000 ) ) ;
#3178 = DIRECTION ( 'NONE',  ( 0.000000000000000000, -1.000000000000000000, -0.000000000000000000 ) ) ;
#3179 = DIRECTION ( 'NONE',  ( 0.000000000000000000, 0.000000000000000000, 1.000000000000000000 ) ) ;
#3180 = EDGE_CURVE ( 'NONE', #11942, #3524, #11188, .T. ) ;
#3181 = DIRECTION ( 'NONE',  ( 0.000000000000000000, 0.000000000000000000, 1.000000000000000000 ) ) ;
#3182 = CARTESIAN_POINT ( 'NONE',  ( 49.99999999999996447, 90.00000000000000000, -8.000000000000000000 ) ) ;
#3183 = APPLICATION_CONTEXT ( 'automotive_design' ) ;
#3184 = FACE_OUTER_BOUND ( 'NONE', #9806, .T. ) ;
#3185 = CARTESIAN_POINT ( 'NONE',  ( 6.500000000000000000, 79.07477288111861924, -1.000000000000000222 ) ) ;
#3186 = CARTESIAN_POINT ( 'NONE',  ( 20.00000000000000355, 121.2009999999999934, 1.500000000000000444 ) ) ;
#3187 = ORIENTED_EDGE ( 'NONE', *, *, #10309, .F. ) ;
#3188 = CARTESIAN_POINT ( 'NONE',  ( -61.00000000000000711, 31.73205080756887142, 3.000000000000000000 ) ) ;
#3189 = ORIENTED_EDGE ( 'NONE', *, *, #10607, .F. ) ;
#3190 =( LENGTH_UNIT ( ) NAMED_UNIT ( * ) SI_UNIT ( .MILLI., .METRE. ) );
#3191 = AXIS2_PLACEMENT_3D ( 'NONE', #3627, #8780, #12773 ) ;
#3192 = DIRECTION ( 'NONE',  ( -1.000000000000000000, 0.000000000000000000, -2.891205793294679312E-17 ) ) ;
#3193 = LINE ( 'NONE', #5074, #6588 ) ;
#3194 = EDGE_CURVE ( 'NONE', #4984, #9287, #12424, .T. ) ;
#3195 = DIRECTION ( 'NONE',  ( -5.624500927088228034E-17, 1.370729058197317775E-18, 1.000000000000000000 ) ) ;
#3196 = ORIENTED_EDGE ( 'NONE', *, *, #10476, .T. ) ;
#3197 = PLANE ( 'NONE',  #4913 ) ;
#3198 = LINE ( 'NONE', #6981, #1034 ) ;
#3199 = ORIENTED_EDGE ( 'NONE', *, *, #1813, .F. ) ;
#3200 = VECTOR ( 'NONE', #10123, 1000.000000000000000 ) ;
#3201 = DIRECTION ( 'NONE',  ( 1.000000000000000000, 0.000000000000000000, -1.390002785237826498E-17 ) ) ;
#3202 = ORIENTED_EDGE ( 'NONE', *, *, #10109, .F. ) ;
#3203 = CARTESIAN_POINT ( 'NONE',  ( 40.00000000000000000, 2.000000000000000000, 10.00000000000000000 ) ) ;
#3204 = VERTEX_POINT ( 'NONE', #3517 ) ;
#3205 = EDGE_CURVE ( 'NONE', #4183, #4549, #6381, .T. ) ;
#3206 = EDGE_CURVE ( 'NONE', #112, #6226, #11352, .T. ) ;
#3207 = CARTESIAN_POINT ( 'NONE',  ( 0.000000000000000000, 0.000000000000000000, 3.000000000000000000 ) ) ;
#3208 = CARTESIAN_POINT ( 'NONE',  ( 1.040000000000000036, -1.154700538379251684, -1.199226976249124676E-17 ) ) ;
#3209 = VERTEX_POINT ( 'NONE', #5530 ) ;
#3210 = PRODUCT_DEFINITION_CONTEXT ( 'detailed design', #2088, 'design' ) ;
#3211 = MECHANICAL_DESIGN_GEOMETRIC_PRESENTATION_REPRESENTATION (  '', ( #2579 ), #12619 ) ;
#3212 = ORIENTED_EDGE ( 'NONE', *, *, #3298, .F. ) ;
#3213 = CARTESIAN_POINT ( 'NONE',  ( 3.800000000000015365, 90.00000000000000000, 3.762500001229034385 ) ) ;
#3214 = VERTEX_POINT ( 'NONE', #2534 ) ;
#3215 = AXIS2_PLACEMENT_3D ( 'NONE', #3235, #329, #4083 ) ;
#3216 = CARTESIAN_POINT ( 'NONE',  ( 50.60000000000001563, 62.98000740192552627, 4.362500001229034474 ) ) ;
#3217 = EDGE_LOOP ( 'NONE', ( #11577, #3476, #4241, #9291, #11148, #12810, #11964, #7077 ) ) ;
#3218 = FACE_OUTER_BOUND ( 'NONE', #10325, .T. ) ;
#3219 = DIRECTION ( 'NONE',  ( -0.8660254037844360431, -0.5000000000000047740, -0.000000000000000000 ) ) ;
#3220 = ORIENTED_EDGE ( 'NONE', *, *, #6904, .T. ) ;
#3221 = CARTESIAN_POINT ( 'NONE',  ( 35.00000000000000000, 90.00000000000000000, 6.000000000000000000 ) ) ;
#3222 = CARTESIAN_POINT ( 'NONE',  ( 3.556430356250014579, 108.1539533981018053, 4.315625000614517148 ) ) ;
#3223 = DIRECTION ( 'NONE',  ( 0.000000000000000000, 0.000000000000000000, -1.000000000000000000 ) ) ;
#3224 = CARTESIAN_POINT ( 'NONE',  ( 50.59999999999999432, 117.0199925980744666, 3.612500001229034474 ) ) ;
#3225 = VECTOR ( 'NONE', #9394, 1000.000000000000000 ) ;
#3226 = SURFACE_STYLE_FILL_AREA ( #11739 ) ;
#3227 = CARTESIAN_POINT ( 'NONE',  ( 19.40000000000002700, 62.98000740192551206, 4.174999999999999822 ) ) ;
#3228 = EDGE_CURVE ( 'NONE', #9676, #1830, #6509, .T. ) ;
#3229 = ORIENTED_EDGE ( 'NONE', *, *, #4593, .T. ) ;
#3230 = CARTESIAN_POINT ( 'NONE',  ( 35.00000000000000711, 53.69209320379640360, 4.521875000614516971 ) ) ;
#3231 = ORIENTED_EDGE ( 'NONE', *, *, #9024, .F. ) ;
#3232 = LINE ( 'NONE', #4274, #9812 ) ;
#3233 = ORIENTED_EDGE ( 'NONE', *, *, #12643, .F. ) ;
#3234 = VECTOR ( 'NONE', #4674, 1000.000000000000000 ) ;
#3235 = CARTESIAN_POINT ( 'NONE',  ( -60.00000000000000000, 30.00000000000000000, 3.000000000000000000 ) ) ;
#3236 = ORIENTED_EDGE ( 'NONE', *, *, #11318, .T. ) ;
#3237 = AXIS2_PLACEMENT_3D ( 'NONE', #8158, #7170, #3126 ) ;
#3238 = CARTESIAN_POINT ( 'NONE',  ( 50.00000000000000000, 121.2009999999999934, -1.500000000000000000 ) ) ;
#3239 = CARTESIAN_POINT ( 'NONE',  ( 35.00000000000000711, 53.69209320379640360, 3.565625000614517592 ) ) ;
#3240 = VERTEX_POINT ( 'NONE', #7653 ) ;
#3241 = DIRECTION ( 'NONE',  ( 0.000000000000000000, 0.000000000000000000, -1.000000000000000000 ) ) ;
#3242 = MANIFOLD_SOLID_BREP ( 'AdvancedHole1', #10097 ) ;
#3243 = LINE ( 'NONE', #1197, #4348 ) ;
#3244 = CARTESIAN_POINT ( 'NONE',  ( 0.000000000000000000, 0.000000000000000000, 0.000000000000000000 ) ) ;
#3245 = AXIS2_PLACEMENT_3D ( 'NONE', #505, #639, #6531 ) ;
#3246 = ADVANCED_FACE ( 'NONE', ( #2494 ), #12566, .T. ) ;
#3247 = VECTOR ( 'NONE', #11468, 1000.000000000000114 ) ;
#3248 = CARTESIAN_POINT ( 'NONE',  ( 48.49999999999995737, 90.00000000000000000, -10.00000000000000000 ) ) ;
#3249 = PLANE ( 'NONE',  #76 ) ;
#3250 = DIRECTION ( 'NONE',  ( 0.000000000000000000, 0.5150380737757255245, 0.8571673013836856869 ) ) ;
#3251 = DIRECTION ( 'NONE',  ( 0.000000000000000000, 0.000000000000000000, 1.000000000000000000 ) ) ;
#3252 = CIRCLE ( 'NONE', #934, 3.349999999999995204 ) ;
#3253 = FACE_OUTER_BOUND ( 'NONE', #12430, .T. ) ;
#3254 = ORIENTED_EDGE ( 'NONE', *, *, #1724, .T. ) ;
#3255 = AXIS2_PLACEMENT_3D ( 'NONE', #1753, #1884, #3920 ) ;
#3256 = DIRECTION ( 'NONE',  ( 0.000000000000000000, 0.000000000000000000, -1.000000000000000000 ) ) ;
#3257 = EDGE_LOOP ( 'NONE', ( #8053, #1252, #2350, #2230 ) ) ;
#3258 = ADVANCED_FACE ( 'NONE', ( #2557 ), #3672, .F. ) ;
#3259 =( NAMED_UNIT ( * ) PLANE_ANGLE_UNIT ( ) SI_UNIT ( $, .RADIAN. ) );
#3260 = EDGE_CURVE ( 'NONE', #41, #3601, #8442, .T. ) ;
#3261 = DIRECTION ( 'NONE',  ( 0.000000000000000000, -1.000000000000000000, 0.000000000000000000 ) ) ;
#3262 = PLANE ( 'NONE',  #11349 ) ;
#3263 = AXIS2_PLACEMENT_3D ( 'NONE', #4676, #7551, #8541 ) ;
#3264 = CYLINDRICAL_SURFACE ( 'NONE', #9272, 1.500000000000001332 ) ;
#3265 = VECTOR ( 'NONE', #12500, 1000.000000000000000 ) ;
#3266 =( BOUNDED_CURVE ( )  B_SPLINE_CURVE ( 2, ( #7463, #7331, #9295, #1179, #12438, #10408, #6220 ),
 .UNSPECIFIED., .F., .F. ) 
 B_SPLINE_CURVE_WITH_KNOTS ( ( 3, 2, 2, 3 ),
 ( 0.5999999999999999778, 0.6333333333333334147, 0.6666666666666667407, 0.7000000000000001776 ),
 .UNSPECIFIED. ) 
 CURVE ( )  GEOMETRIC_REPRESENTATION_ITEM ( )  RATIONAL_B_SPLINE_CURVE ( ( 1.000000000000000000, 0.8660254037844387076, 1.000000000000000000, 0.8660254037844387076, 1.000000000000000000, 0.8660254037844378194, 1.000000000000000888 ) ) 
 REPRESENTATION_ITEM ( '' )  );
#3267 = ORIENTED_EDGE ( 'NONE', *, *, #7224, .F. ) ;
#3268 = CARTESIAN_POINT ( 'NONE',  ( 50.00000000000000000, 0.000000000000000000, -10.00000000000000000 ) ) ;
#3269 = CARTESIAN_POINT ( 'NONE',  ( 41.31805916882746033, 91.52713075379783447, -1.000000000000000000 ) ) ;
#3270 = ORIENTED_EDGE ( 'NONE', *, *, #11837, .T. ) ;
#3271 =( LENGTH_UNIT ( ) NAMED_UNIT ( * ) SI_UNIT ( .MILLI., .METRE. ) );
#3272 = DIRECTION ( 'NONE',  ( 0.000000000000000000, -0.000000000000000000, 1.000000000000000000 ) ) ;
#3273 = ORIENTED_EDGE ( 'NONE', *, *, #464, .F. ) ;
#3274 = ORIENTED_EDGE ( 'NONE', *, *, #4879, .F. ) ;
#3275 = ADVANCED_FACE ( 'NONE', ( #2623 ), #1501, .F. ) ;
#3276 = AXIS2_PLACEMENT_3D ( 'NONE', #1418, #10641, #1618 ) ;
#3277 = DIRECTION ( 'NONE',  ( 0.000000000000000000, 1.000000000000000000, 0.000000000000000000 ) ) ;
#3278 = LINE ( 'NONE', #8501, #8740 ) ;
#3279 = ORIENTED_EDGE ( 'NONE', *, *, #10746, .T. ) ;
#3280 = VERTEX_POINT ( 'NONE', #509 ) ;
#3281 = DIRECTION ( 'NONE',  ( -0.8660254037844397068, -0.4999999999999985567, -0.000000000000000000 ) ) ;
#3282 = ORIENTED_EDGE ( 'NONE', *, *, #4843, .F. ) ;
#3283 = APPLICATION_PROTOCOL_DEFINITION ( 'draft international standard', 'automotive_design', 1998, #1241 ) ;
#3284 = CARTESIAN_POINT ( 'NONE',  ( 66.44356964374999563, 71.84604660189820891, 3.640625000614517326 ) ) ;
#3285 = EDGE_CURVE ( 'NONE', #9018, #9939, #11443, .T. ) ;
#3286 = VECTOR ( 'NONE', #9449, 1000.000000000000000 ) ;
#3287 = EDGE_LOOP ( 'NONE', ( #508, #7957, #6808, #12755 ) ) ;
#3288 = DIRECTION ( 'NONE',  ( -0.000000000000000000, 1.000000000000000000, -0.000000000000000000 ) ) ;
#3289 = ORIENTED_EDGE ( 'NONE', *, *, #8865, .F. ) ;
#3290 = DIRECTION ( 'NONE',  ( 0.000000000000000000, 0.000000000000000000, 1.000000000000000000 ) ) ;
#3291 = CARTESIAN_POINT ( 'NONE',  ( 50.60000000000001563, 62.98000740192552627, 4.700000000000000178 ) ) ;
#3292 = CARTESIAN_POINT ( 'NONE',  ( 3.800000000000025135, 71.98667160128366049, 3.350000001229034297 ) ) ;
#3293 = AXIS2_PLACEMENT_3D ( 'NONE', #9096, #10705, #3658 ) ;
#3294 = DIRECTION ( 'NONE',  ( 1.000000000000000000, 0.000000000000000000, 0.000000000000000000 ) ) ;
#3295 = ORIENTED_EDGE ( 'NONE', *, *, #10929, .F. ) ;
#3296 = CARTESIAN_POINT ( 'NONE',  ( 50.60000000000001563, 62.98000740192552627, 4.250000000000000000 ) ) ;
#3297 = ORIENTED_EDGE ( 'NONE', *, *, #5990, .T. ) ;
#3298 = EDGE_CURVE ( 'NONE', #8873, #5463, #10657, .T. ) ;
#3299 = CARTESIAN_POINT ( 'NONE',  ( 60.32621597448488870, 111.4045591870091840, 3.026619673138257749 ) ) ;
#3300 = EDGE_LOOP ( 'NONE', ( #6905, #12091, #10348, #6277 ) ) ;
#3301 = EDGE_CURVE ( 'NONE', #587, #6336, #5487, .T. ) ;
#3302 = DIRECTION ( 'NONE',  ( -0.000000000000000000, -0.000000000000000000, 1.000000000000000000 ) ) ;
#3303 = ORIENTED_EDGE ( 'NONE', *, *, #1765, .T. ) ;
#3304 = AXIS2_PLACEMENT_3D ( 'NONE', #3188, #12206, #7237 ) ;
#3305 = CARTESIAN_POINT ( 'NONE',  ( 44.16515138991168499, 86.00000000000000000, -10.00000000000000000 ) ) ;
#3306 = CARTESIAN_POINT ( 'NONE',  ( 19.27821517812500574, 117.2309300971526937, 4.278125000614516615 ) ) ;
#3307 = CARTESIAN_POINT ( 'NONE',  ( 35.00000000000000711, 53.69209320379639649, 3.621875000614517059 ) ) ;
#3308 = MANIFOLD_SOLID_BREP ( 'AdvancedHole1', #1951 ) ;
#3309 = DIRECTION ( 'NONE',  ( 1.049727191973305517E-16, 0.5150380737757253025, -0.8571673013836857979 ) ) ;
#3310 = FACE_BOUND ( 'NONE', #1957, .T. ) ;
#3311 = VECTOR ( 'NONE', #10618, 1000.000000000000000 ) ;
#3312 = CARTESIAN_POINT ( 'NONE',  ( 9.999999999999994671, 30.00000000000000000, 2.500000000000000000 ) ) ;
#3313 = CARTESIAN_POINT ( 'NONE',  ( -6.666666666666660745, 0.000000000000000000, -1.599999999999998090 ) ) ;
#3314 = CARTESIAN_POINT ( 'NONE',  ( 9.294992700730281499, 72.31688376601880464, -1.000000000000000000 ) ) ;
#3315 = DIRECTION ( 'NONE',  ( 0.000000000000000000, 0.000000000000000000, 1.000000000000000000 ) ) ;
#3316 = FACE_OUTER_BOUND ( 'NONE', #7620, .T. ) ;
#3317 = CARTESIAN_POINT ( 'NONE',  ( 66.44356964374999563, 90.00000000000000000, 3.734375000614516882 ) ) ;
#3318 = ADVANCED_FACE ( 'NONE', ( #893 ), #5748, .F. ) ;
#3319 = VECTOR ( 'NONE', #5863, 1000.000000000000000 ) ;
#3320 = ORIENTED_EDGE ( 'NONE', *, *, #3554, .T. ) ;
#3321 = DIRECTION ( 'NONE',  ( -1.000000000000000000, 0.000000000000000000, -5.337610695313252124E-17 ) ) ;
#3322 = ORIENTED_EDGE ( 'NONE', *, *, #2636, .F. ) ;
#3323 = CARTESIAN_POINT ( 'NONE',  ( 35.00000000000000000, 90.00000000000000000, 6.000000000000000000 ) ) ;
#3324 = PLANE ( 'NONE',  #7178 ) ;
#3325 = VECTOR ( 'NONE', #7351, 1000.000000000000000 ) ;
#3326 = UNCERTAINTY_MEASURE_WITH_UNIT (LENGTH_MEASURE( 1.000000000000000082E-05 ), #11835, 'distance_accuracy_value', 'NONE');
#3327 = ORIENTED_EDGE ( 'NONE', *, *, #12071, .F. ) ;
#3328 = EDGE_CURVE ( 'NONE', #1894, #4333, #10846, .T. ) ;
#3329 = CARTESIAN_POINT ( 'NONE',  ( 45.00000000000000000, 2.000000000000001332, 7.349999999999990763 ) ) ;
#3330 = DIRECTION ( 'NONE',  ( -1.000000000000000000, -0.000000000000000000, -0.000000000000000000 ) ) ;
#3331 = EDGE_CURVE ( 'NONE', #11426, #10133, #5874, .T. ) ;
#3332 = ORIENTED_EDGE ( 'NONE', *, *, #4614, .F. ) ;
#3333 = SURFACE_SIDE_STYLE ('',( #1288 ) ) ;
#3334 = LINE ( 'NONE', #2221, #750 ) ;
#3335 = ADVANCED_FACE ( 'NONE', ( #1827 ), #2880, .F. ) ;
#3336 = EDGE_LOOP ( 'NONE', ( #5339, #10851, #11204, #8554 ) ) ;
#3337 = VECTOR ( 'NONE', #7159, 1000.000000000000114 ) ;
#3338 = VERTEX_POINT ( 'NONE', #772 ) ;
#3339 = AXIS2_PLACEMENT_3D ( 'NONE', #1913, #664, #12654 ) ;
#3340 = PLANE ( 'NONE',  #4245 ) ;
#3341 = DIRECTION ( 'NONE',  ( 0.000000000000000000, -1.000000000000000000, 0.000000000000000000 ) ) ;
#3342 = ORIENTED_EDGE ( 'NONE', *, *, #7158, .T. ) ;
#3343 =( BOUNDED_CURVE ( )  B_SPLINE_CURVE ( 2, ( #8606, #11608, #4547, #11669, #3827, #11803, #5589 ),
 .UNSPECIFIED., .F., .F. ) 
 B_SPLINE_CURVE_WITH_KNOTS ( ( 3, 2, 2, 3 ),
 ( 0.5999999999999999778, 0.6333333333333334147, 0.6666666666666667407, 0.7000000000000001776 ),
 .UNSPECIFIED. ) 
 CURVE ( )  GEOMETRIC_REPRESENTATION_ITEM ( )  RATIONAL_B_SPLINE_CURVE ( ( 1.000000000000000000, 0.8660254037844387076, 1.000000000000000000, 0.8660254037844387076, 1.000000000000000000, 0.8660254037844378194, 1.000000000000000888 ) ) 
 REPRESENTATION_ITEM ( '' )  );
#3344 = ORIENTED_EDGE ( 'NONE', *, *, #8568, .T. ) ;
#3346 = DIRECTION ( 'NONE',  ( -0.000000000000000000, -0.000000000000000000, -1.000000000000000000 ) ) ;
#3345 = CIRCLE ( 'NONE', #9182, 1.599999999999997202 ) ;
#3347 = ORIENTED_EDGE ( 'NONE', *, *, #10558, .T. ) ;
#3348 = DIRECTION ( 'NONE',  ( 0.3957342950827466566, 0.000000000000000000, 0.9183650514339936066 ) ) ;
#3349 = CARTESIAN_POINT ( 'NONE',  ( 3.556430356250015024, 90.00000000000000000, 3.003125000614517148 ) ) ;
#3350 = EDGE_CURVE ( 'NONE', #5561, #8524, #1890, .T. ) ;
#3351 = ORIENTED_EDGE ( 'NONE', *, *, #1911, .F. ) ;
#3352 = CARTESIAN_POINT ( 'NONE',  ( 35.75000000000000711, 92.49999999999998579, -9.802775637731997449 ) ) ;
#3353 = EDGE_LOOP ( 'NONE', ( #11829, #2799, #43, #6095 ) ) ;
#3354 = CARTESIAN_POINT ( 'NONE',  ( 3.800000000000015365, 90.00000000000000000, 4.100000000000000533 ) ) ;
#3355 = CARTESIAN_POINT ( 'NONE',  ( 3.800000000000039790, 71.98667160128364628, 4.587500000000000355 ) ) ;
#3356 = AXIS2_PLACEMENT_3D ( 'NONE', #9673, #12880, #10843 ) ;
#3357 = CARTESIAN_POINT ( 'NONE',  ( -53.33333333333332149, 33.84900179459754810, 3.000000000000000000 ) ) ;
#3358 = CARTESIAN_POINT ( 'NONE',  ( -2.387319993259524598, -4.036502139894371233, -0.8000000000000000444 ) ) ;
#3359 = EDGE_LOOP ( 'NONE', ( #2722, #6802, #5417, #5440 ) ) ;
#3360 = CARTESIAN_POINT ( 'NONE',  ( 3.556430356250028790, 71.84604660189818048, 3.546875000614516882 ) ) ;
#3361 = CARTESIAN_POINT ( 'NONE',  ( -48.33333333333332860, 0.000000000000000000, -1.734723475976807094E-15 ) ) ;
#3362 = ADVANCED_FACE ( 'NONE', ( #9995 ), #9730, .F. ) ;
#3363 = VERTEX_POINT ( 'NONE', #9006 ) ;
#3364 = AXIS2_PLACEMENT_3D ( 'NONE', #12072, #8085, #1072 ) ;
#3365 = VECTOR ( 'NONE', #11635, 1000.000000000000000 ) ;
#3366 = FACE_BOUND ( 'NONE', #3064, .T. ) ;
#3367 = ORIENTED_EDGE ( 'NONE', *, *, #7399, .T. ) ;
#3368 = DIRECTION ( 'NONE',  ( -0.000000000000000000, 1.000000000000000000, -0.000000000000000000 ) ) ;
#3369 = DIRECTION ( 'NONE',  ( -1.000000000000000000, -0.000000000000000000, -0.000000000000000000 ) ) ;
#3370 = CARTESIAN_POINT ( 'NONE',  ( 0.000000000000000000, -1.154700538379251684, -1.199226976249124676E-17 ) ) ;
#3371 = LINE ( 'NONE', #598, #9575 ) ;
#3372 = EDGE_CURVE ( 'NONE', #11106, #5904, #4899, .T. ) ;
#3373 = CARTESIAN_POINT ( 'NONE',  ( 9.294992700730281499, 72.31688376601880464, 5.000000000000000000 ) ) ;
#3374 = ADVANCED_FACE ( 'NONE', ( #12812 ), #9741, .F. ) ;
#3375 = VECTOR ( 'NONE', #4085, 1000.000000000000000 ) ;
#3376 = DIRECTION ( 'NONE',  ( 0.000000000000000000, 0.000000000000000000, 1.000000000000000000 ) ) ;
#3377 = DIRECTION ( 'NONE',  ( 8.673617379884034486E-16, 0.000000000000000000, -1.000000000000000000 ) ) ;
#3378 = PLANE ( 'NONE',  #3753 ) ;
#3379 = CARTESIAN_POINT ( 'NONE',  ( 48.49999999999995737, 90.00000000000000000, -8.000000000000000000 ) ) ;
#3380 = CARTESIAN_POINT ( 'NONE',  ( 1.040000000000000036, -1.154700538379251684, -1.199226976249124676E-17 ) ) ;
#3381 = AXIS2_PLACEMENT_3D ( 'NONE', #10864, #2833, #11974 ) ;
#3382 = CARTESIAN_POINT ( 'NONE',  ( 52.44898870156725224, 66.83414752204051013, -1.000000000000000222 ) ) ;
#3383 = EDGE_LOOP ( 'NONE', ( #1967, #230, #5298 ) ) ;
#3384 = PLANE ( 'NONE',  #6419 ) ;
#3385 = ORIENTED_EDGE ( 'NONE', *, *, #8109, .T. ) ;
#3386 = MANIFOLD_SOLID_BREP ( 'Cavity1', #7803 ) ;
#3387 = PRESENTATION_LAYER_ASSIGNMENT (  '', '', ( #12157 ) ) ;
#3388 = CARTESIAN_POINT ( 'NONE',  ( 35.00000000000000000, 90.00000000000000000, 1.000000000000003109 ) ) ;
#3389 = DIRECTION ( 'NONE',  ( 0.000000000000000000, 0.000000000000000000, 1.000000000000000000 ) ) ;
#3390 = EDGE_CURVE ( 'NONE', #1413, #11262, #2941, .T. ) ;
#3391 = CARTESIAN_POINT ( 'NONE',  ( -61.00000000000000711, 31.73205080756887142, 0.9999999999999926725 ) ) ;
#3392 = ORIENTED_EDGE ( 'NONE', *, *, #3205, .T. ) ;
#3393 = DIRECTION ( 'NONE',  ( -0.000000000000000000, -0.000000000000000000, -1.000000000000000000 ) ) ;
#3394 = CARTESIAN_POINT ( 'NONE',  ( 35.00000000000000000, 90.00000000000000000, 4.000000000000000000 ) ) ;
#3395 = ORIENTED_EDGE ( 'NONE', *, *, #8879, .T. ) ;
#3396 = CARTESIAN_POINT ( 'NONE',  ( 0.000000000000000000, 0.5773502691896262862, 1.000000000000000000 ) ) ;
#3397 = EDGE_LOOP ( 'NONE', ( #10965, #5431, #5265, #7983, #392 ) ) ;
#3398 = ORIENTED_EDGE ( 'NONE', *, *, #5677, .F. ) ;
#3399 = CARTESIAN_POINT ( 'NONE',  ( 3.800000000000135270, 108.0133283987163679, 2.825000001229033941 ) ) ;
#3400 = CARTESIAN_POINT ( 'NONE',  ( 20.00000000000000355, 2.000000000000001776, -1.499999999999999556 ) ) ;
#3401 = EDGE_CURVE ( 'NONE', #10264, #1821, #1954, .T. ) ;
#3402 = ORIENTED_EDGE ( 'NONE', *, *, #12032, .T. ) ;
#3403 = ADVANCED_FACE ( 'NONE', ( #7841 ), #3070, .F. ) ;
#3404 = ORIENTED_EDGE ( 'NONE', *, *, #11539, .F. ) ;
#3405 = VECTOR ( 'NONE', #2945, 1000.000000000000000 ) ;
#3406 = DIRECTION ( 'NONE',  ( 0.000000000000000000, 0.000000000000000000, 1.000000000000000000 ) ) ;
#3407 = ORIENTED_EDGE ( 'NONE', *, *, #5709, .F. ) ;
#3408 = CARTESIAN_POINT ( 'NONE',  ( 35.16468375597256824, 121.3570802786415328, 3.000000000000001332 ) ) ;
#3409 = SHAPE_DEFINITION_REPRESENTATION ( #2399, #2422 ) ;
#3410 = CARTESIAN_POINT ( 'NONE',  ( 66.19999999999997442, 108.0133283987163253, 3.575000001229033941 ) ) ;
#3411 = ORIENTED_EDGE ( 'NONE', *, *, #7459, .T. ) ;
#3412 = CARTESIAN_POINT ( 'NONE',  ( 25.00000000000000355, -5.000000000000000000, 5.750000000000000000 ) ) ;
#3413 = EDGE_LOOP ( 'NONE', ( #12358, #9333, #11344, #12552 ) ) ;
#3414 = DIRECTION ( 'NONE',  ( -1.000000000000000000, 0.000000000000000000, 0.000000000000000000 ) ) ;
#3415 = CARTESIAN_POINT ( 'NONE',  ( 35.00000000000000711, 53.97334320256736362, 4.662499999999999645 ) ) ;
#3416 = CARTESIAN_POINT ( 'NONE',  ( 53.69851220231782207, 63.41305505666788633, 1.000000000000003109 ) ) ;
#3417 =( NAMED_UNIT ( * ) PLANE_ANGLE_UNIT ( ) SI_UNIT ( $, .RADIAN. ) );
#3418 = ADVANCED_FACE ( 'NONE', ( #7050 ), #101, .F. ) ;
#3419 = VERTEX_POINT ( 'NONE', #12351 ) ;
#3420 = CARTESIAN_POINT ( 'NONE',  ( 66.44356964374999563, 90.00000000000000000, 3.284375000614517148 ) ) ;
#3421 = VERTEX_POINT ( 'NONE', #10054 ) ;
#3422 = DIRECTION ( 'NONE',  ( -1.000000000000000000, 0.000000000000000000, -5.337610695313252124E-17 ) ) ;
#3423 =( GEOMETRIC_REPRESENTATION_CONTEXT ( 3 ) GLOBAL_UNCERTAINTY_ASSIGNED_CONTEXT ( ( #8007 ) ) GLOBAL_UNIT_ASSIGNED_CONTEXT ( ( #7207, #3417, #11193 ) ) REPRESENTATION_CONTEXT ( 'NONE', 'WORKASPACE' ) );
#3424 = CARTESIAN_POINT ( 'NONE',  ( 50.72178482187501203, 62.76906990284730625, 4.559375000614517504 ) ) ;
#3425 = ORIENTED_EDGE ( 'NONE', *, *, #11602, .T. ) ;
#3426 = DIRECTION ( 'NONE',  ( -8.673617379884035472E-16, -5.007715329123921945E-16, -1.000000000000000000 ) ) ;
#3427 = AXIS2_PLACEMENT_3D ( 'NONE', #1857, #8851, #10876 ) ;
#3428 = DIRECTION ( 'NONE',  ( 0.000000000000000000, 0.000000000000000000, -1.000000000000000000 ) ) ;
#3429 = DIRECTION ( 'NONE',  ( 0.000000000000000000, 0.000000000000000000, 1.000000000000000000 ) ) ;
#3430 = FACE_OUTER_BOUND ( 'NONE', #3744, .T. ) ;
#3431 =( REPRESENTATION_RELATIONSHIP ('NONE','NONE', #1997, #985 ) REPRESENTATION_RELATIONSHIP_WITH_TRANSFORMATION ( #1696 )SHAPE_REPRESENTATION_RELATIONSHIP( ) );
#3432 = EDGE_CURVE ( 'NONE', #1735, #485, #8230, .T. ) ;
#3433 = DIRECTION ( 'NONE',  ( 0.000000000000000000, 0.000000000000000000, 1.000000000000000000 ) ) ;
#3434 = COLOUR_RGB ( '',1.000000000000000000, 0.9490196078431372140, 0.9098039215686274384 ) ;
#3435 = FACE_OUTER_BOUND ( 'NONE', #4962, .T. ) ;
#3436 = FACE_OUTER_BOUND ( 'NONE', #9725, .T. ) ;
#3437 = CLOSED_SHELL ( 'NONE', ( #11559, #4000, #4960, #11672, #2678, #4536, #8783, #4670, #6197, #9442, #2193, #11247, #12663, #8303, #3246, #7961, #7011, #7239, #11712, #12, #10976, #1604, #9427, #5787, #2621, #4785, #10788 ) ) ;
#3438 = FACE_OUTER_BOUND ( 'NONE', #1550, .T. ) ;
#3439 = DIRECTION ( 'NONE',  ( -0.000000000000000000, -0.000000000000000000, 1.000000000000000000 ) ) ;
#3440 = VECTOR ( 'NONE', #10110, 1000.000000000000000 ) ;
#3441 = CYLINDRICAL_SURFACE ( 'NONE', #9516, 1.499999999999999556 ) ;
#3442 = EDGE_CURVE ( 'NONE', #12578, #2627, #4371, .T. ) ;
#3443 = EDGE_CURVE ( 'NONE', #1735, #9892, #1289, .T. ) ;
#3444 = CARTESIAN_POINT ( 'NONE',  ( 63.99885733073620742, 89.74256357754359215, -0.9999999999999970024 ) ) ;
#3445 = CARTESIAN_POINT ( 'NONE',  ( 20.00000000000000355, 0.000000000000000000, 10.00000000000000000 ) ) ;
#3446 = ORIENTED_EDGE ( 'NONE', *, *, #7865, .T. ) ;
#3447 = DIRECTION ( 'NONE',  ( 1.000000000000000000, 0.000000000000000000, 0.000000000000000000 ) ) ;
#3448 = DIRECTION ( 'NONE',  ( 0.000000000000000000, 0.000000000000000000, 1.000000000000000000 ) ) ;
#3449 = ORIENTED_EDGE ( 'NONE', *, *, #12633, .F. ) ;
#3450 = AXIS2_PLACEMENT_3D ( 'NONE', #6445, #12403, #1676 ) ;
#3451 = EDGE_CURVE ( 'NONE', #5692, #10832, #2011, .T. ) ;
#3452 = CARTESIAN_POINT ( 'NONE',  ( 38.40477530926830951, 84.46307801270444315, 22.38477631085024555 ) ) ;
#3453 = CARTESIAN_POINT ( 'NONE',  ( 3.800000000000015365, 90.00000000000000000, 4.212500001229034119 ) ) ;
#3454 = FACE_OUTER_BOUND ( 'NONE', #4254, .T. ) ;
#3455 = EDGE_LOOP ( 'NONE', ( #10721, #12724, #9171, #8954 ) ) ;
#3456 = VECTOR ( 'NONE', #3792, 1000.000000000000114 ) ;
#3457 = CARTESIAN_POINT ( 'NONE',  ( -38.66666666666665719, 30.00000000000000000, 7.999999999999996447 ) ) ;
#3458 = LINE ( 'NONE', #12348, #10863 ) ;
#3459 = EDGE_CURVE ( 'NONE', #3150, #7702, #5281, .T. ) ;
#3460 = CIRCLE ( 'NONE', #10117, 1.599999999999998757 ) ;
#3461 = VERTEX_POINT ( 'NONE', #4246 ) ;
#3462 = CARTESIAN_POINT ( 'NONE',  ( 0.000000000000000000, 0.000000000000000000, 0.000000000000000000 ) ) ;
#3463 = CYLINDRICAL_SURFACE ( 'NONE', #4936, 4.999999999999997335 ) ;
#3464 = ORIENTED_EDGE ( 'NONE', *, *, #9180, .T. ) ;
#3465 = CARTESIAN_POINT ( 'NONE',  ( 1.040000000000000036, 0.000000000000000000, 2.000000000000000000 ) ) ;
#3466 = EDGE_LOOP ( 'NONE', ( #12289, #7761, #5875, #696 ) ) ;
#3467 = CARTESIAN_POINT ( 'NONE',  ( -0.1038759689922479496, -3.348389132562988646, 0.000000000000000000 ) ) ;
#3468 = FACE_OUTER_BOUND ( 'NONE', #3902, .T. ) ;
#3469 = VECTOR ( 'NONE', #12282, 1000.000000000000000 ) ;
#3470 = ORIENTED_EDGE ( 'NONE', *, *, #5652, .F. ) ;
#3471 = ORIENTED_EDGE ( 'NONE', *, *, #16, .F. ) ;
#3472 = FACE_OUTER_BOUND ( 'NONE', #2024, .T. ) ;
#3473 = VERTEX_POINT ( 'NONE', #1088 ) ;
#3474 = CYLINDRICAL_SURFACE ( 'NONE', #8252, 30.00000000000000000 ) ;
#3475 = CARTESIAN_POINT ( 'NONE',  ( 19.40000000000000924, 117.0199925980744666, 4.587500001229034119 ) ) ;
#3476 = ORIENTED_EDGE ( 'NONE', *, *, #390, .F. ) ;
#3477 = AXIS2_PLACEMENT_3D ( 'NONE', #5325, #12069, #9186 ) ;
#3478 = DIRECTION ( 'NONE',  ( 0.8660254037844361541, 0.5000000000000042188, 0.000000000000000000 ) ) ;
#3479 = VERTEX_POINT ( 'NONE', #7312 ) ;
#3480 = VECTOR ( 'NONE', #6054, 1000.000000000000114 ) ;
#3481 = ORIENTED_EDGE ( 'NONE', *, *, #426, .F. ) ;
#3482 = EDGE_CURVE ( 'NONE', #11236, #955, #3334, .T. ) ;
#3483 = CARTESIAN_POINT ( 'NONE',  ( 0.000000000000000000, 0.4117131682837005258, -0.8000000000000000444 ) ) ;
#3484 = PLANE ( 'NONE',  #11871 ) ;
#3485 = UNCERTAINTY_MEASURE_WITH_UNIT (LENGTH_MEASURE( 1.000000000000000082E-05 ), #761, 'distance_accuracy_value', 'NONE');
#3486 = ORIENTED_EDGE ( 'NONE', *, *, #10138, .T. ) ;
#3487 = CONICAL_SURFACE ( 'NONE', #5138, 1.219500000000000028, 0.7853981633974463916 ) ;
#3488 = LINE ( 'NONE', #3871, #11383 ) ;
#3489 = VERTEX_POINT ( 'NONE', #11296 ) ;
#3490 = CARTESIAN_POINT ( 'NONE',  ( 66.19999999999998863, 90.00000000000000000, 3.087500001229034119 ) ) ;
#3491 = ORIENTED_EDGE ( 'NONE', *, *, #7233, .T. ) ;
#3492 = CARTESIAN_POINT ( 'NONE',  ( 3.556430356250028790, 71.84604660189818048, 3.546875000614516882 ) ) ;
#3493 = EDGE_LOOP ( 'NONE', ( #9077, #8307, #2879, #673 ) ) ;
#3494 = EDGE_CURVE ( 'NONE', #12299, #10459, #2440, .T. ) ;
#3495 = FACE_OUTER_BOUND ( 'NONE', #10612, .T. ) ;
#3496 = CARTESIAN_POINT ( 'NONE',  ( 5.000000000000004441, 30.00000000000000000, 10.00000000000000000 ) ) ;
#3497 = EDGE_CURVE ( 'NONE', #8511, #2940, #3060, .T. ) ;
#3498 = AXIS2_PLACEMENT_3D ( 'NONE', #12393, #474, #5590 ) ;
#3499 = CARTESIAN_POINT ( 'NONE',  ( 66.44356964374998142, 108.1539533981018053, 3.321875000614517237 ) ) ;
#3500 = CARTESIAN_POINT ( 'NONE',  ( -57.99999999999999289, 2.000000000000000000, 7.999999999999996447 ) ) ;
#3501 = DIRECTION ( 'NONE',  ( 1.000000000000000000, 0.000000000000000000, 0.000000000000000000 ) ) ;
#3502 = DIRECTION ( 'NONE',  ( -0.5877852522924753575, 0.8090169943749458970, 0.000000000000000000 ) ) ;
#3503 = DIRECTION ( 'NONE',  ( 1.000000000000000000, 2.135044278125301343E-15, 0.000000000000000000 ) ) ;
#3504 = DIRECTION ( 'NONE',  ( -0.8660254037844393737, -0.4999999999999987232, 0.000000000000000000 ) ) ;
#3505 = LINE ( 'NONE', #7614, #7612 ) ;
#3506 = AXIS2_PLACEMENT_3D ( 'NONE', #11285, #4103, #10303 ) ;
#3507 = CARTESIAN_POINT ( 'NONE',  ( 35.00000000000000000, 90.00000000000000000, -3.799999999999999822 ) ) ;
#3508 = ADVANCED_FACE ( 'NONE', ( #9074 ), #229, .F. ) ;
#3509 = CARTESIAN_POINT ( 'NONE',  ( 66.19999999999998863, 90.00000000000000000, 4.774999999999999467 ) ) ;
#3510 = DIRECTION ( 'NONE',  ( -0.000000000000000000, -0.000000000000000000, -1.000000000000000000 ) ) ;
#3511 = VERTEX_POINT ( 'NONE', #10318 ) ;
#3512 = CARTESIAN_POINT ( 'NONE',  ( 65.00000000000000000, 90.00000000000000000, -0.9999999999999970024 ) ) ;
#3513 = DIRECTION ( 'NONE',  ( 0.8660254037844361541, 0.5000000000000042188, 0.000000000000000000 ) ) ;
#3514 = VERTEX_POINT ( 'NONE', #1352 ) ;
#3515 = AXIS2_PLACEMENT_3D ( 'NONE', #10372, #675, #8547 ) ;
#3516 = LINE ( 'NONE', #9651, #7615 ) ;
#3517 = CARTESIAN_POINT ( 'NONE',  ( -56.02330673931587768, 34.91474707805760858, 0.000000000000000000 ) ) ;
#3518 = CARTESIAN_POINT ( 'NONE',  ( 35.00000000000000000, 90.00000000000000000, 5.000000000000000000 ) ) ;
#3519 = ORIENTED_EDGE ( 'NONE', *, *, #10138, .F. ) ;
#3520 = DIRECTION ( 'NONE',  ( -0.3262398754384822630, 0.9452870165584014162, 0.000000000000000000 ) ) ;
#3521 = CIRCLE ( 'NONE', #11239, 1.500000000000002665 ) ;
#3522 = CARTESIAN_POINT ( 'NONE',  ( 66.44356964375000985, 71.84604660189820891, 4.540625000614517681 ) ) ;
#3523 = VECTOR ( 'NONE', #11007, 1000.000000000000114 ) ;
#3524 = VERTEX_POINT ( 'NONE', #5343 ) ;
#3525 = DIRECTION ( 'NONE',  ( 0.000000000000000000, -1.000000000000000000, 0.000000000000000000 ) ) ;
#3526 = VERTEX_POINT ( 'NONE', #3396 ) ;
#3527 = CARTESIAN_POINT ( 'NONE',  ( 64.31840955652157277, 100.6710290542226574, 3.000000000000000000 ) ) ;
#3528 = ORIENTED_EDGE ( 'NONE', *, *, #2794, .F. ) ;
#3529 = LINE ( 'NONE', #4636, #677 ) ;
#3530 = DIRECTION ( 'NONE',  ( 0.000000000000000000, 0.5150380737757253025, 0.8571673013836857979 ) ) ;
#3531 = ORIENTED_EDGE ( 'NONE', *, *, #4345, .T. ) ;
#3532 = EDGE_CURVE ( 'NONE', #485, #11942, #6179, .T. ) ;
#3533 = AXIS2_PLACEMENT_3D ( 'NONE', #6458, #2352, #4506 ) ;
#3534 = ADVANCED_FACE ( 'NONE', ( #12154 ), #11233, .F. ) ;
#3535 = VERTEX_POINT ( 'NONE', #12088 ) ;
#3536 = CARTESIAN_POINT ( 'NONE',  ( 34.25000000000000000, 93.26496554346289258, -3.799999999999999822 ) ) ;
#3537 = ORIENTED_EDGE ( 'NONE', *, *, #7500, .F. ) ;
#3538 = CARTESIAN_POINT ( 'NONE',  ( -60.00000000000000000, 30.00000000000000000, 3.000000000000000000 ) ) ;
#3539 = CARTESIAN_POINT ( 'NONE',  ( 50.59999999999999432, 117.0199925980744666, 4.512500001229033941 ) ) ;
#3541 = MANIFOLD_SOLID_BREP ( 'Hex', #5303 ) ;
#3540 = ORIENTED_EDGE ( 'NONE', *, *, #12418, .F. ) ;
#3542 = PRESENTATION_STYLE_ASSIGNMENT (( #5623 ) ) ;
#3543 = ORIENTED_EDGE ( 'NONE', *, *, #2598, .F. ) ;
#3544 = CARTESIAN_POINT ( 'NONE',  ( 36.50000000000001421, 67.79999999999999716, 8.000000000000000000 ) ) ;
#3545 = ORIENTED_EDGE ( 'NONE', *, *, #3949, .F. ) ;
#3546 = DIRECTION ( 'NONE',  ( 0.000000000000000000, 0.000000000000000000, -1.000000000000000000 ) ) ;
#3547 = PLANE ( 'NONE',  #6006 ) ;
#3548 = VECTOR ( 'NONE', #10623, 1000.000000000000000 ) ;
#3549 = PRODUCT_RELATED_PRODUCT_CATEGORY ( 'part', '', ( #4379 ) ) ;
#3550 = VECTOR ( 'NONE', #4412, 1000.000000000000000 ) ;
#3551 = VERTEX_POINT ( 'NONE', #8560 ) ;
#3552 = CARTESIAN_POINT ( 'NONE',  ( 3.556430356250028790, 71.84604660189818048, 3.096875000614517592 ) ) ;
#3553 = ORIENTED_EDGE ( 'NONE', *, *, #12602, .T. ) ;
#3554 = EDGE_CURVE ( 'NONE', #5411, #10403, #11409, .T. ) ;
#3555 = CARTESIAN_POINT ( 'NONE',  ( 7.500000000000000000, 34.99999999999999289, 0.000000000000000000 ) ) ;
#3556 = ORIENTED_EDGE ( 'NONE', *, *, #5161, .T. ) ;
#3557 = CARTESIAN_POINT ( 'NONE',  ( 50.72178482187499071, 117.2309300971526937, 3.809375000614517504 ) ) ;
#3558 = ORIENTED_EDGE ( 'NONE', *, *, #3170, .F. ) ;
#3559 = CIRCLE ( 'NONE', #6250, 1.499999999999999556 ) ;
#3560 = DIRECTION ( 'NONE',  ( 1.000000000000000000, 0.000000000000000000, 0.000000000000000000 ) ) ;
#3561 = FACE_OUTER_BOUND ( 'NONE', #5545, .T. ) ;
#3562 = DIRECTION ( 'NONE',  ( -1.000000000000000000, 0.000000000000000000, 0.000000000000000000 ) ) ;
#3563 = CARTESIAN_POINT ( 'NONE',  ( 66.19999999999998863, 90.00000000000000000, 3.087500001229034119 ) ) ;
#3564 = CARTESIAN_POINT ( 'NONE',  ( 66.20000000000000284, 90.00000000000000000, 6.000000000000000000 ) ) ;
#3565 = EDGE_CURVE ( 'NONE', #2419, #2737, #11624, .T. ) ;
#3566 = CARTESIAN_POINT ( 'NONE',  ( 45.00000000000000000, 0.000000000000000000, 5.750000000000000888 ) ) ;
#3567 = AXIS2_PLACEMENT_3D ( 'NONE', #3587, #1615, #8296 ) ;
#3568 = LINE ( 'NONE', #2580, #8461 ) ;
#3569 = ADVANCED_FACE ( 'NONE', ( #6582 ), #3487, .T. ) ;
#3570 = FACE_OUTER_BOUND ( 'NONE', #10154, .T. ) ;
#3571 = FACE_OUTER_BOUND ( 'NONE', #2559, .T. ) ;
#3572 = CARTESIAN_POINT ( 'NONE',  ( 31.96709571323326671, 88.25314809233525182, -3.799999999999999378 ) ) ;
#3573 = CARTESIAN_POINT ( 'NONE',  ( 66.19999999999998863, 90.00000000000000000, 4.437500001229033764 ) ) ;
#3574 = LINE ( 'NONE', #9581, #11628 ) ;
#3575 = ORIENTED_EDGE ( 'NONE', *, *, #9520, .F. ) ;
#3576 = FACE_OUTER_BOUND ( 'NONE', #9791, .T. ) ;
#3577 = CARTESIAN_POINT ( 'NONE',  ( -57.55384757729342482, 35.76313972081443637, 1.836970198721030427E-16 ) ) ;
#3578 = ORIENTED_EDGE ( 'NONE', *, *, #1544, .T. ) ;
#3579 = SURFACE_SIDE_STYLE ('',( #12537 ) ) ;
#3580 = EDGE_CURVE ( 'NONE', #10434, #7702, #9464, .T. ) ;
#3581 = LINE ( 'NONE', #1611, #6563 ) ;
#3582 = DIRECTION ( 'NONE',  ( 0.8958148394926558344, 0.4444274669107966536, 4.977592430910269431E-17 ) ) ;
#3583 = CARTESIAN_POINT ( 'NONE',  ( 35.49992570027444572, 118.9956906159209069, 2.000000000000002220 ) ) ;
#3584 = AXIS2_PLACEMENT_3D ( 'NONE', #8462, #2188, #4341 ) ;
#3585 = EDGE_LOOP ( 'NONE', ( #3003, #11479, #10078, #8240 ) ) ;
#3586 = LINE ( 'NONE', #8737, #1785 ) ;
#3587 = CARTESIAN_POINT ( 'NONE',  ( 0.000000000000000000, 0.000000000000000000, -10.00000000000000000 ) ) ;
#3588 = EDGE_LOOP ( 'NONE', ( #1764, #5107, #298, #3083 ) ) ;
#3589 = FACE_OUTER_BOUND ( 'NONE', #9409, .T. ) ;
#3590 = CARTESIAN_POINT ( 'NONE',  ( 48.49999999999995737, 90.00000000000000000, -10.00000000000000178 ) ) ;
#3591 = ORIENTED_EDGE ( 'NONE', *, *, #2127, .T. ) ;
#3592 = LINE ( 'NONE', #1745, #4331 ) ;
#3593 = ORIENTED_EDGE ( 'NONE', *, *, #7780, .F. ) ;
#3594 = LINE ( 'NONE', #7576, #30 ) ;
#3595 = VECTOR ( 'NONE', #9157, 1000.000000000000000 ) ;
#3596 = DIRECTION ( 'NONE',  ( -1.000000000000000000, 0.000000000000000000, 0.000000000000000000 ) ) ;
#3597 = ADVANCED_FACE ( 'NONE', ( #4567 ), #7443, .T. ) ;
#3598 = CARTESIAN_POINT ( 'NONE',  ( 35.00000000000000000, 90.00000000000000000, -3.000000000000000000 ) ) ;
#3599 = VERTEX_POINT ( 'NONE', #11425 ) ;
#3600 = DIRECTION ( 'NONE',  ( 0.000000000000000000, -0.000000000000000000, 1.000000000000000000 ) ) ;
#3601 = VERTEX_POINT ( 'NONE', #2541 ) ;
#3602 = CARTESIAN_POINT ( 'NONE',  ( -60.00000000000000000, 23.99999999999998934, 2.500000000000000000 ) ) ;
#3603 = APPLICATION_PROTOCOL_DEFINITION ( 'draft international standard', 'automotive_design', 1998, #55 ) ;
#3604 = CARTESIAN_POINT ( 'NONE',  ( 66.19999999999998863, 90.00000000000000000, 3.987500001229034030 ) ) ;
#3605 = ORIENTED_EDGE ( 'NONE', *, *, #7854, .F. ) ;
#3606 =( REPRESENTATION_RELATIONSHIP ('NONE','NONE', #1997, #9014 ) REPRESENTATION_RELATIONSHIP_WITH_TRANSFORMATION ( #8378 )SHAPE_REPRESENTATION_RELATIONSHIP( ) );
#3607 = EDGE_CURVE ( 'NONE', #8571, #7199, #9322, .T. ) ;
#3608 = ORIENTED_EDGE ( 'NONE', *, *, #1382, .T. ) ;
#3609 = EDGE_CURVE ( 'NONE', #11688, #9045, #1172, .T. ) ;
#3610 =( NAMED_UNIT ( * ) PLANE_ANGLE_UNIT ( ) SI_UNIT ( $, .RADIAN. ) );
#3611 = ORIENTED_EDGE ( 'NONE', *, *, #9460, .F. ) ;
#3612 = CARTESIAN_POINT ( 'NONE',  ( 25.31483199390188332, 60.14306353880185441, 3.000000000000001332 ) ) ;
#3613 = CARTESIAN_POINT ( 'NONE',  ( 35.00000000000000000, 90.00000000000000000, -8.000000000000000000 ) ) ;
#3614 = UNCERTAINTY_MEASURE_WITH_UNIT (LENGTH_MEASURE( 1.000000000000000082E-05 ), #2042, 'distance_accuracy_value', 'NONE');
#3615 = AXIS2_PLACEMENT_3D ( 'NONE', #8531, #12518, #1655 ) ;
#3616 = EDGE_CURVE ( 'NONE', #11952, #955, #1593, .T. ) ;
#3617 = ORIENTED_EDGE ( 'NONE', *, *, #4217, .F. ) ;
#3618 = CARTESIAN_POINT ( 'NONE',  ( 3.556430356250015024, 90.00000000000000000, 3.059375000614517059 ) ) ;
#3619 = ORIENTED_EDGE ( 'NONE', *, *, #7084, .F. ) ;
#3620 = DIRECTION ( 'NONE',  ( -0.000000000000000000, -0.000000000000000000, -1.000000000000000000 ) ) ;
#3621 = ORIENTED_EDGE ( 'NONE', *, *, #8569, .F. ) ;
#3622 = CARTESIAN_POINT ( 'NONE',  ( 35.00000000000000711, 53.69209320379640360, 3.621875000614517059 ) ) ;
#3623 = ORIENTED_EDGE ( 'NONE', *, *, #3285, .T. ) ;
#3624 = VECTOR ( 'NONE', #711, 999.9999999999998863 ) ;
#3625 = DIRECTION ( 'NONE',  ( 1.000000000000000000, 0.000000000000000000, 0.000000000000000000 ) ) ;
#3626 = CARTESIAN_POINT ( 'NONE',  ( -0.9999999999999997780, -4.273461295629625845, -0.8000000000000000444 ) ) ;
#3627 = CARTESIAN_POINT ( 'NONE',  ( 35.00000000000000000, 90.00000000000000000, 4.800000000000000711 ) ) ;
#3628 = CARTESIAN_POINT ( 'NONE',  ( 66.44356964374998142, 108.1539533981018053, 4.615625000614516971 ) ) ;
#3629 = EDGE_CURVE ( 'NONE', #9137, #9525, #4696, .T. ) ;
#3630 = CARTESIAN_POINT ( 'NONE',  ( 31.86869970978804290, 88.80942934165229019, 4.800000000000000711 ) ) ;
#3631 =( GEOMETRIC_REPRESENTATION_CONTEXT ( 3 ) GLOBAL_UNCERTAINTY_ASSIGNED_CONTEXT ( ( #12637 ) ) GLOBAL_UNIT_ASSIGNED_CONTEXT ( ( #2073, #8874, #882 ) ) REPRESENTATION_CONTEXT ( 'NONE', 'WORKASPACE' ) );
#3632 = DIRECTION ( 'NONE',  ( 1.000000000000000000, 0.000000000000000000, 0.000000000000000000 ) ) ;
#3633 = DIRECTION ( 'NONE',  ( 0.2967717757331703732, -0.9549484348006340717, -0.000000000000000000 ) ) ;
#3634 = CARTESIAN_POINT ( 'NONE',  ( 34.49999999999995026, 119.0000000000000000, 4.000000000000000000 ) ) ;
#3635 = VECTOR ( 'NONE', #2013, 1000.000000000000000 ) ;
#3636 = DIRECTION ( 'NONE',  ( 0.000000000000000000, 1.000000000000000000, 1.224646799147353207E-16 ) ) ;
#3637 = CARTESIAN_POINT ( 'NONE',  ( 35.00000000000000000, 90.00000000000000000, 5.000000000000000000 ) ) ;
#3638 = CARTESIAN_POINT ( 'NONE',  ( 35.00000000000000000, 90.00000000000000000, -3.000000000000000888 ) ) ;
#3639 = ORIENTED_EDGE ( 'NONE', *, *, #1361, .F. ) ;
#3641 = CARTESIAN_POINT ( 'NONE',  ( 50.60000000000001563, 62.98000740192552627, 4.250000000000000000 ) ) ;
#3640 = MECHANICAL_DESIGN_GEOMETRIC_PRESENTATION_REPRESENTATION (  '', ( #268 ), #11772 ) ;
#3642 = CARTESIAN_POINT ( 'NONE',  ( 1.040000000000000036, 0.8660254037844391517, -0.5000000000000006661 ) ) ;
#3643 = EDGE_LOOP ( 'NONE', ( #6511, #7441, #4312, #2495 ) ) ;
#3644 = ADVANCED_FACE ( 'NONE', ( #5539 ), #6516, .F. ) ;
#3645 = AXIS2_PLACEMENT_3D ( 'NONE', #1752, #8628, #12622 ) ;
#3646 = CARTESIAN_POINT ( 'NONE',  ( 1.040000000000000036, 1.154700538379252350, 7.017607234860990640E-28 ) ) ;
#3647 = DIRECTION ( 'NONE',  ( 0.000000000000000000, 0.000000000000000000, 1.000000000000000000 ) ) ;
#3648 = EDGE_LOOP ( 'NONE', ( #10909, #10304, #10244, #6824 ) ) ;
#3649 = VERTEX_POINT ( 'NONE', #1484 ) ;
#3650 = LINE ( 'NONE', #10580, #6575 ) ;
#3651 = CARTESIAN_POINT ( 'NONE',  ( 19.27821517812500574, 117.2309300971526937, 4.278125000614516615 ) ) ;
#3652 = DIRECTION ( 'NONE',  ( -0.000000000000000000, 1.000000000000000000, -0.000000000000000000 ) ) ;
#3653 = AXIS2_PLACEMENT_3D ( 'NONE', #2329, #2266, #1134 ) ;
#3654 = CARTESIAN_POINT ( 'NONE',  ( 9.650000000000000355, 0.000000000000000000, 0.000000000000000000 ) ) ;
#3655 = ORIENTED_EDGE ( 'NONE', *, *, #2223, .T. ) ;
#3656 = EDGE_CURVE ( 'NONE', #7660, #3168, #7634, .T. ) ;
#3657 = VECTOR ( 'NONE', #2857, 1000.000000000000114 ) ;
#3658 = DIRECTION ( 'NONE',  ( 1.000000000000000000, 0.000000000000000000, 0.000000000000000000 ) ) ;
#3659 = ORIENTED_EDGE ( 'NONE', *, *, #3165, .T. ) ;
#3660 = EDGE_CURVE ( 'NONE', #7199, #8571, #6601, .T. ) ;
#3661 = DIRECTION ( 'NONE',  ( -0.000000000000000000, 1.000000000000000000, -0.000000000000000000 ) ) ;
#3662 = DIRECTION ( 'NONE',  ( 0.000000000000000000, 0.000000000000000000, 1.000000000000000000 ) ) ;
#3663 = LINE ( 'NONE', #9607, #608 ) ;
#3664 = VECTOR ( 'NONE', #3439, 1000.000000000000000 ) ;
#3665 = CARTESIAN_POINT ( 'NONE',  ( 35.49999999999999289, 96.48074069840785683, -1.000000000000000000 ) ) ;
#3666 = VECTOR ( 'NONE', #857, 1000.000000000000000 ) ;
#3667 = LINE ( 'NONE', #9859, #2501 ) ;
#3668 = EDGE_LOOP ( 'NONE', ( #2888, #2572, #5845, #3411, #7997, #6613 ) ) ;
#3669 = DIRECTION ( 'NONE',  ( 1.000000000000000000, 0.000000000000000000, 0.000000000000000000 ) ) ;
#3670 = CARTESIAN_POINT ( 'NONE',  ( -60.00000000000000000, 23.99999999999998934, -2.500000000000000000 ) ) ;
#3671 = ORIENTED_EDGE ( 'NONE', *, *, #7104, .T. ) ;
#3672 = CYLINDRICAL_SURFACE ( 'NONE', #5338, 31.19999999999999929 ) ;
#3673 = ORIENTED_EDGE ( 'NONE', *, *, #931, .F. ) ;
#3674 = EDGE_CURVE ( 'NONE', #5295, #2281, #8425, .T. ) ;
#3675 = FILL_AREA_STYLE_COLOUR ( '', #5663 ) ;
#3677 = EDGE_LOOP ( 'NONE', ( #12034, #1914, #1567, #5850 ) ) ;
#3676 = CIRCLE ( 'NONE', #5753, 1.599999999999986766 ) ;
#3678 = VECTOR ( 'NONE', #12166, 1000.000000000000000 ) ;
#3679 = CARTESIAN_POINT ( 'NONE',  ( 45.39999948872177526, 60.58435772187547030, 3.000000000000000000 ) ) ;
#3680 = CARTESIAN_POINT ( 'NONE',  ( 66.19999999999988916, 71.98667160128361786, 3.387499999999999734 ) ) ;
#3682 = ADVANCED_FACE ( 'NONE', ( #2670 ), #3463, .F. ) ;
#3681 = ORIENTED_EDGE ( 'NONE', *, *, #756, .T. ) ;
#3683 = DIRECTION ( 'NONE',  ( -1.000000000000000000, 0.000000000000000000, 0.000000000000000000 ) ) ;
#3684 = EDGE_LOOP ( 'NONE', ( #4513, #2497, #526, #11444, #4882, #8285, #9279, #10500 ) ) ;
#3685 = VECTOR ( 'NONE', #6965, 1000.000000000000000 ) ;
#3686 = LINE ( 'NONE', #6676, #12740 ) ;
#3687 = MECHANICAL_DESIGN_GEOMETRIC_PRESENTATION_REPRESENTATION (  '', ( #8479 ), #10973 ) ;
#3688 = VERTEX_POINT ( 'NONE', #9659 ) ;
#3689 = CARTESIAN_POINT ( 'NONE',  ( 19.27821517812503060, 62.76906990284727783, 4.034375000614517148 ) ) ;
#3690 = ORIENTED_EDGE ( 'NONE', *, *, #3026, .F. ) ;
#3691 = CARTESIAN_POINT ( 'NONE',  ( 0.000000000000000000, 0.4117131682837005258, 0.000000000000000000 ) ) ;
#3692 = DIRECTION ( 'NONE',  ( 0.000000000000000000, 0.000000000000000000, 1.000000000000000000 ) ) ;
#3693 = CARTESIAN_POINT ( 'NONE',  ( 66.44356964374999563, 90.00000000000000000, 3.228125000614517237 ) ) ;
#3694 = AXIS2_PLACEMENT_3D ( 'NONE', #361, #12286, #3201 ) ;
#3695 = CARTESIAN_POINT ( 'NONE',  ( 0.1038759689922479496, -3.348389132562988646, 0.000000000000000000 ) ) ;
#3696 = EDGE_CURVE ( 'NONE', #9525, #4047, #3715, .T. ) ;
#3697 = EDGE_CURVE ( 'NONE', #10418, #5137, #7506, .T. ) ;
#3698 = DIRECTION ( 'NONE',  ( -1.000000000000000000, 0.000000000000000000, 0.000000000000000000 ) ) ;
#3699 = FACE_OUTER_BOUND ( 'NONE', #3107, .T. ) ;
#3700 = DIRECTION ( 'NONE',  ( -1.000000000000000000, -0.000000000000000000, -0.000000000000000000 ) ) ;
#3701 = CARTESIAN_POINT ( 'NONE',  ( 0.000000000000000000, -6.000000000000000000, 0.000000000000000000 ) ) ;
#3702 = CIRCLE ( 'NONE', #10992, 32.70000000000000995 ) ;
#3703 = CARTESIAN_POINT ( 'NONE',  ( 35.00000000000000000, 90.00000000000000000, -3.000000000000000000 ) ) ;
#3704 = CARTESIAN_POINT ( 'NONE',  ( 35.00000000000000711, 53.69209320379640360, 3.621875000614517059 ) ) ;
#3705 = ORIENTED_EDGE ( 'NONE', *, *, #2166, .F. ) ;
#3706 = CARTESIAN_POINT ( 'NONE',  ( 66.20000000000000284, 71.98667160128370313, 4.737500000000000711 ) ) ;
#3707 = ORIENTED_EDGE ( 'NONE', *, *, #8684, .F. ) ;
#3708 = VECTOR ( 'NONE', #5799, 1000.000000000000000 ) ;
#3709 = CARTESIAN_POINT ( 'NONE',  ( 52.44898842787294768, 66.83414752756172561, 4.000000000000000000 ) ) ;
#3710 = DIRECTION ( 'NONE',  ( 0.000000000000000000, 0.5150380737757253025, 0.8571673013836857979 ) ) ;
#3711 = CARTESIAN_POINT ( 'NONE',  ( 21.49999999999998579, 94.00000000000000000, -10.00000000000000000 ) ) ;
#3712 = EDGE_CURVE ( 'NONE', #10832, #5993, #6903, .T. ) ;
#3713 = CARTESIAN_POINT ( 'NONE',  ( 35.00000000000000711, 53.69209320379639649, 3.565625000614517592 ) ) ;
#3714 = CARTESIAN_POINT ( 'NONE',  ( 6.499999999999998224, 68.39379290111055809, 0.9999999999999995559 ) ) ;
#3715 = LINE ( 'NONE', #7699, #10578 ) ;
#3716 = EDGE_LOOP ( 'NONE', ( #4851, #7192, #157, #7403 ) ) ;
#3717 = VECTOR ( 'NONE', #3513, 1000.000000000000114 ) ;
#3718 = LINE ( 'NONE', #9601, #2030 ) ;
#3719 = EDGE_LOOP ( 'NONE', ( #4310, #7882, #3528, #9496 ) ) ;
#3720 = CARTESIAN_POINT ( 'NONE',  ( 35.00000000000000711, 53.97334320256736362, 3.875000001229034208 ) ) ;
#3721 = PLANE ( 'NONE',  #7706 ) ;
#3722 = CARTESIAN_POINT ( 'NONE',  ( 1.040000000000000036, 0.000000000000000000, 0.000000000000000000 ) ) ;
#3723 = EDGE_CURVE ( 'NONE', #1862, #919, #9954, .T. ) ;
#3724 = EDGE_CURVE ( 'NONE', #7344, #11587, #3972, .T. ) ;
#3725 = EDGE_LOOP ( 'NONE', ( #11303, #6580, #1876, #6450 ) ) ;
#3726 = AXIS2_PLACEMENT_3D ( 'NONE', #8336, #8271, #138 ) ;
#3727 = PLANE ( 'NONE',  #9381 ) ;
#3728 = ORIENTED_EDGE ( 'NONE', *, *, #8075, .T. ) ;
#3729 = DIRECTION ( 'NONE',  ( -0.000000000000000000, -0.000000000000000000, -1.000000000000000000 ) ) ;
#3730 = ADVANCED_FACE ( 'NONE', ( #8869 ), #11879, .F. ) ;
#3731 = LINE ( 'NONE', #3794, #6887 ) ;
#3732 = EDGE_LOOP ( 'NONE', ( #8175, #2147, #11196, #6726, #10411, #4835 ) ) ;
#3733 =( NAMED_UNIT ( * ) SI_UNIT ( $, .STERADIAN. ) SOLID_ANGLE_UNIT ( ) );
#3734 = ORIENTED_EDGE ( 'NONE', *, *, #5652, .T. ) ;
#3735 = CARTESIAN_POINT ( 'NONE',  ( -1.625004804578467077, -6.241943558307533557, -0.8000000000000000444 ) ) ;
#3736 = EDGE_LOOP ( 'NONE', ( #11765, #10718, #6111, #12335 ) ) ;
#3737 = AXIS2_PLACEMENT_3D ( 'NONE', #3722, #2549, #12559 ) ;
#3738 = AXIS2_PLACEMENT_3D ( 'NONE', #11773, #10793, #12635 ) ;
#3739 = LINE ( 'NONE', #12757, #3624 ) ;
#3740 = CARTESIAN_POINT ( 'NONE',  ( 41.00904217445251732, 92.47818727009297390, -0.9999999999999970024 ) ) ;
#3741 = EDGE_CURVE ( 'NONE', #7875, #10050, #5731, .T. ) ;
#3742 = ORIENTED_EDGE ( 'NONE', *, *, #9802, .T. ) ;
#3743 = DIRECTION ( 'NONE',  ( 0.000000000000000000, 0.000000000000000000, 1.000000000000000000 ) ) ;
#3744 = EDGE_LOOP ( 'NONE', ( #2875, #4769, #2119, #6842 ) ) ;
#3745 = CARTESIAN_POINT ( 'NONE',  ( 35.00000000000000000, 90.00000000000000000, 4.800000000000000711 ) ) ;
#3746 = AXIS2_PLACEMENT_3D ( 'NONE', #1459, #1522, #5512 ) ;
#3747 = VERTEX_POINT ( 'NONE', #2796 ) ;
#3748 = CARTESIAN_POINT ( 'NONE',  ( 35.00000000000000000, 126.3079067962035822, 2.890625000614516882 ) ) ;
#3749 = ORIENTED_EDGE ( 'NONE', *, *, #9088, .T. ) ;
#3750 = CARTESIAN_POINT ( 'NONE',  ( 20.00000000000000355, 62.64236852357281293, 5.000000000000000000 ) ) ;
#3751 = DIRECTION ( 'NONE',  ( 1.000000000000000000, 0.000000000000000000, 0.000000000000000000 ) ) ;
#3752 = CARTESIAN_POINT ( 'NONE',  ( 9.294992700730283275, 72.31688376601880464, 1.000000000000000000 ) ) ;
#3753 = AXIS2_PLACEMENT_3D ( 'NONE', #272, #7354, #1946 ) ;
#3754 = CARTESIAN_POINT ( 'NONE',  ( 66.44356964374999563, 71.84604660189820891, 4.090625000614517504 ) ) ;
#3755 = AXIS2_PLACEMENT_3D ( 'NONE', #3566, #601, #3376 ) ;
#3756 = CARTESIAN_POINT ( 'NONE',  ( 35.00000000000000000, 90.00000000000000000, -1.000000000000000000 ) ) ;
#3757 = EDGE_CURVE ( 'NONE', #11429, #10403, #5915, .T. ) ;
#3758 = DIRECTION ( 'NONE',  ( -1.000000000000000000, 0.000000000000000000, 0.000000000000000000 ) ) ;
#3759 = CARTESIAN_POINT ( 'NONE',  ( 3.800000000000015365, 90.00000000000000000, 4.549999999999999822 ) ) ;
#3760 = CARTESIAN_POINT ( 'NONE',  ( 0.000000000000000000, 0.000000000000000000, -0.8000000000000000444 ) ) ;
#3761 = VECTOR ( 'NONE', #9303, 1000.000000000000000 ) ;
#3762 = FACE_OUTER_BOUND ( 'NONE', #12367, .T. ) ;
#3763 = LINE ( 'NONE', #7553, #4411 ) ;
#3764 = CARTESIAN_POINT ( 'NONE',  ( 35.00000000000000000, 126.3079067962035822, 2.946875000614516793 ) ) ;
#3766 = ADVANCED_FACE ( 'NONE', ( #9913 ), #3841, .T. ) ;
#3765 = VERTEX_POINT ( 'NONE', #9722 ) ;
#3767 = ADVANCED_FACE ( 'NONE', ( #5982 ), #7890, .T. ) ;
#3768 = CARTESIAN_POINT ( 'NONE',  ( 3.800000000000015365, 108.0133283987163111, 4.512500000000000178 ) ) ;
#3769 = CARTESIAN_POINT ( 'NONE',  ( 50.59999999999999432, 117.0199925980744666, 3.612500001229034474 ) ) ;
#3770 = ORIENTED_EDGE ( 'NONE', *, *, #3301, .F. ) ;
#3771 = PRODUCT_DEFINITION_SHAPE ( 'NONE', 'NONE',  #12963 ) ;
#3772 = VECTOR ( 'NONE', #833, 1000.000000000000000 ) ;
#3773 = PLANE ( 'NONE',  #10329 ) ;
#3774 = PLANE ( 'NONE',  #9282 ) ;
#3775 = CARTESIAN_POINT ( 'NONE',  ( -15.06519709809452756, 92.38262548349219117, 1.000000000000003109 ) ) ;
#3776 = CARTESIAN_POINT ( 'NONE',  ( 35.00000000000000000, 126.3079067962036106, 3.340625000614517504 ) ) ;
#3777 = VECTOR ( 'NONE', #6628, 1000.000000000000000 ) ;
#3779 = VECTOR ( 'NONE', #4224, 1000.000000000000114 ) ;
#3778 = LINE ( 'NONE', #11748, #6485 ) ;
#3780 = CARTESIAN_POINT ( 'NONE',  ( 65.00000000000000000, 117.5000000000001705, 1.000000000000003109 ) ) ;
#3781 = EDGE_LOOP ( 'NONE', ( #11836, #8051, #348, #12465, #2414, #196, #9565, #9483 ) ) ;
#3782 = CARTESIAN_POINT ( 'NONE',  ( -60.00000000000000000, 0.000000000000000000, 14.99999999999999645 ) ) ;
#3783 = ORIENTED_EDGE ( 'NONE', *, *, #5308, .T. ) ;
#3784 = FACE_BOUND ( 'NONE', #4596, .T. ) ;
#3785 = EDGE_CURVE ( 'NONE', #10285, #11420, #11501, .T. ) ;
#3786 = VECTOR ( 'NONE', #5903, 1000.000000000000000 ) ;
#3787 = DIRECTION ( 'NONE',  ( 0.000000000000000000, 0.000000000000000000, 1.000000000000000000 ) ) ;
#3788 = LINE ( 'NONE', #5989, #10306 ) ;
#3789 = DIRECTION ( 'NONE',  ( -0.8090169943749485615, 0.5877852522924716938, 0.000000000000000000 ) ) ;
#3790 = LINE ( 'NONE', #7769, #11042 ) ;
#3791 = VERTEX_POINT ( 'NONE', #12140 ) ;
#3792 = DIRECTION ( 'NONE',  ( 0.03100775193798453039, -0.9995191440486532741, 0.000000000000000000 ) ) ;
#3793 = ITEM_DEFINED_TRANSFORMATION ( 'NONE', 'NONE', #9696,  #5704 ) ;
#3794 = CARTESIAN_POINT ( 'NONE',  ( -60.00000000000000000, 0.000000000000000000, -10.00000000000000355 ) ) ;
#3795 = ORIENTED_EDGE ( 'NONE', *, *, #4878, .F. ) ;
#3796 =( NAMED_UNIT ( * ) PLANE_ANGLE_UNIT ( ) SI_UNIT ( $, .RADIAN. ) );
#3797 = ORIENTED_EDGE ( 'NONE', *, *, #10741, .F. ) ;
#3798 = VECTOR ( 'NONE', #12583, 999.9999999999998863 ) ;
#3799 = EDGE_CURVE ( 'NONE', #10113, #6517, #12073, .T. ) ;
#3800 = CARTESIAN_POINT ( 'NONE',  ( 6.499999999999999112, 70.70319397786906279, 3.000000000000039080 ) ) ;
#3801 = ORIENTED_EDGE ( 'NONE', *, *, #2598, .T. ) ;
#3802 = CARTESIAN_POINT ( 'NONE',  ( 17.32445633083897008, 64.11686499059005939, 3.000000000000001776 ) ) ;
#3803 = FACE_OUTER_BOUND ( 'NONE', #4909, .T. ) ;
#3804 = EDGE_CURVE ( 'NONE', #1692, #7167, #2868, .T. ) ;
#3805 = ORIENTED_EDGE ( 'NONE', *, *, #938, .F. ) ;
#3806 = DIRECTION ( 'NONE',  ( 1.049727191973304038E-16, -0.5150380737757271898, 0.8571673013836847987 ) ) ;
#3807 = ORIENTED_EDGE ( 'NONE', *, *, #4521, .F. ) ;
#3808 = CARTESIAN_POINT ( 'NONE',  ( 48.49999999999995737, 90.00000000000000000, -10.00000000000000000 ) ) ;
#3809 = ORIENTED_EDGE ( 'NONE', *, *, #9698, .F. ) ;
#3810 = CARTESIAN_POINT ( 'NONE',  ( 3.556430356250014579, 108.1539533981018053, 3.415625000614517237 ) ) ;
#3811 = VERTEX_POINT ( 'NONE', #2134 ) ;
#3812 = CYLINDRICAL_SURFACE ( 'NONE', #5256, 1.599999999999992539 ) ;
#3813 = CARTESIAN_POINT ( 'NONE',  ( 5.000000000000004441, 0.000000000000000000, -10.00000000000000000 ) ) ;
#3814 = ADVANCED_FACE ( 'NONE', ( #9190 ), #12006, .T. ) ;
#3815 = VECTOR ( 'NONE', #10074, 1000.000000000000000 ) ;
#3816 = CARTESIAN_POINT ( 'NONE',  ( 66.20000000000000284, 71.98667160128370313, 3.950000001229034829 ) ) ;
#3817 = ADVANCED_FACE ( 'NONE', ( #9254 ), #11147, .F. ) ;
#3818 = B_SPLINE_CURVE_WITH_KNOTS ( 'NONE', 3,
 ( #4354, #9189, #12463, #3382 ),
 .UNSPECIFIED., .F., .F.,
 ( 4, 4 ),
 ( 0.000000000000000000, 1.000000000000000000 ),
 .UNSPECIFIED. ) ;
#3819 = DIRECTION ( 'NONE',  ( 0.000000000000000000, -0.8660254037844384856, 0.5000000000000003331 ) ) ;
#3820 = CARTESIAN_POINT ( 'NONE',  ( -31.49999999999998579, 46.45448267190452185, -1.000000000000000000 ) ) ;
#3821 = CARTESIAN_POINT ( 'NONE',  ( 28.50000000000000355, 90.00000000000000000, -1.000000000000000888 ) ) ;
#3822 = CARTESIAN_POINT ( 'NONE',  ( 35.75000000000000711, 93.41869858279433458, 22.38477631085024555 ) ) ;
#3823 = DIRECTION ( 'NONE',  ( -1.000000000000000000, -0.000000000000000000, -0.000000000000000000 ) ) ;
#3824 = AXIS2_PLACEMENT_3D ( 'NONE', #1294, #2291, #5284 ) ;
#3825 = CARTESIAN_POINT ( 'NONE',  ( 64.54728994471078352, 100.7543353520590870, 2.802601390178781404 ) ) ;
#3826 = VERTEX_POINT ( 'NONE', #6181 ) ;
#3827 = CARTESIAN_POINT ( 'NONE',  ( 50.59999999999999432, 117.0199925980744666, 3.500000000000000444 ) ) ;
#3828 = CARTESIAN_POINT ( 'NONE',  ( 19.27821517812503060, 62.76906990284727783, 4.034375000614517148 ) ) ;
#3829 = ORIENTED_EDGE ( 'NONE', *, *, #1902, .T. ) ;
#3830 = EDGE_CURVE ( 'NONE', #7336, #11940, #3054, .T. ) ;
#3831 = CARTESIAN_POINT ( 'NONE',  ( 66.19999999999997442, 108.0133283987163253, 3.912500000000000533 ) ) ;
#3832 = CARTESIAN_POINT ( 'NONE',  ( -9.666666666666657193, 59.05996354921150271, 1.000000000000000000 ) ) ;
#3833 = VERTEX_POINT ( 'NONE', #8282 ) ;
#3834 = DIRECTION ( 'NONE',  ( -1.000000000000000000, 0.000000000000000000, 0.000000000000000000 ) ) ;
#3835 = AXIS2_PLACEMENT_3D ( 'NONE', #4953, #5739, #4765 ) ;
#3836 = CARTESIAN_POINT ( 'NONE',  ( 7.266925296109192800, 98.48530998897412303, -1.000000000000000000 ) ) ;
#3837 = EDGE_CURVE ( 'NONE', #4305, #7601, #1138, .T. ) ;
#3838 = CARTESIAN_POINT ( 'NONE',  ( 52.49999999999996447, 86.00000000000000000, -8.000000000000000000 ) ) ;
#3839 = CARTESIAN_POINT ( 'NONE',  ( 50.72178482187501203, 62.76906990284730625, 3.603125000614517681 ) ) ;
#3840 = CARTESIAN_POINT ( 'NONE',  ( 25.00000000000000355, 2.000000000000001332, 7.349999999999986322 ) ) ;
#3841 = PLANE ( 'NONE',  #12680 ) ;
#3842 = VERTEX_POINT ( 'NONE', #1334 ) ;
#3843 = CARTESIAN_POINT ( 'NONE',  ( 7.500000000000000000, 27.00000000000000000, -1.599999999999992095 ) ) ;
#3844 = VERTEX_POINT ( 'NONE', #9324 ) ;
#3845 = VECTOR ( 'NONE', #10634, 1000.000000000000227 ) ;
#3846 = EDGE_CURVE ( 'NONE', #10533, #1140, #4115, .T. ) ;
#3847 =( NAMED_UNIT ( * ) PLANE_ANGLE_UNIT ( ) SI_UNIT ( $, .RADIAN. ) );
#3848 = FACE_OUTER_BOUND ( 'NONE', #8032, .T. ) ;
#3849 = PRODUCT_DEFINITION_FORMATION_WITH_SPECIFIED_SOURCE ( 'ANY', '', #1339, .NOT_KNOWN. ) ;
#3850 = PLANE ( 'NONE',  #10621 ) ;
#3851 = DIRECTION ( 'NONE',  ( -1.000000000000000000, 0.000000000000000000, 0.000000000000000000 ) ) ;
#3852 = FACE_OUTER_BOUND ( 'NONE', #3413, .T. ) ;
#3853 = ADVANCED_FACE ( 'NONE', ( #2069 ), #6047, .T. ) ;
#3854 = DIRECTION ( 'NONE',  ( -0.000000000000000000, -0.000000000000000000, -1.000000000000000000 ) ) ;
#3855 = EDGE_LOOP ( 'NONE', ( #5618, #10401, #10940, #8946, #12770, #11323, #326, #12436, #7505, #2725, #1616, #8763 ) ) ;
#3856 = AXIS2_PLACEMENT_3D ( 'NONE', #1869, #9972, #11743 ) ;
#3857 = DIRECTION ( 'NONE',  ( -1.000000000000000000, -0.000000000000000000, -0.000000000000000000 ) ) ;
#3858 = ITEM_DEFINED_TRANSFORMATION ( 'NONE', 'NONE', #7810,  #5704 ) ;
#3859 = CARTESIAN_POINT ( 'NONE',  ( 50.00000000000000000, 2.000000000000000000, 10.00000000000000000 ) ) ;
#3860 = AXIS2_PLACEMENT_3D ( 'NONE', #12668, #1475, #4688 ) ;
#3861 = VERTEX_POINT ( 'NONE', #212 ) ;
#3862 = DIRECTION ( 'NONE',  ( -1.000000000000000000, 0.000000000000000000, 0.000000000000000000 ) ) ;
#3863 = EDGE_LOOP ( 'NONE', ( #10855, #7117 ) ) ;
#3864 = CARTESIAN_POINT ( 'NONE',  ( 20.00000000000000355, 2.000000000000001776, -1.499999999999999556 ) ) ;
#3865 = ORIENTED_EDGE ( 'NONE', *, *, #1307, .T. ) ;
#3866 = CARTESIAN_POINT ( 'NONE',  ( 52.49999999999996447, 86.00000000000000000, -10.00000000000000000 ) ) ;
#3867 = CARTESIAN_POINT ( 'NONE',  ( 3.799999999999904787, 71.98667160128373155, 3.237499999999999822 ) ) ;
#3868 = VECTOR ( 'NONE', #9831, 1000.000000000000000 ) ;
#3869 = AXIS2_PLACEMENT_3D ( 'NONE', #4414, #8404, #2454 ) ;
#3870 = ORIENTED_EDGE ( 'NONE', *, *, #2400, .T. ) ;
#3871 = CARTESIAN_POINT ( 'NONE',  ( 31.86464806177570352, 88.44450386581220869, 6.000000000000000000 ) ) ;
#3872 = PRODUCT_DEFINITION ( 'UNKNOWN', '', #708, #2420 ) ;
#3873 = EDGE_LOOP ( 'NONE', ( #4568, #3055, #189, #611 ) ) ;
#3874 = DIRECTION ( 'NONE',  ( -0.000000000000000000, -0.000000000000000000, -1.000000000000000000 ) ) ;
#3875 = ORIENTED_EDGE ( 'NONE', *, *, #1710, .T. ) ;
#3876 = CIRCLE ( 'NONE', #8476, 0.5999999999999998668 ) ;
#3877 = CARTESIAN_POINT ( 'NONE',  ( 19.27821517812500574, 117.2309300971526937, 3.828125000614516882 ) ) ;
#3878 = ADVANCED_FACE ( 'NONE', ( #3253 ), #6110, .T. ) ;
#3879 = ORIENTED_EDGE ( 'NONE', *, *, #4878, .T. ) ;
#3880 = AXIS2_PLACEMENT_3D ( 'NONE', #9475, #503, #4641 ) ;
#3881 = LINE ( 'NONE', #5040, #10887 ) ;
#3882 = CARTESIAN_POINT ( 'NONE',  ( 25.00000000000000355, 2.000000000000001332, -7.349999999999986322 ) ) ;
#3883 = CARTESIAN_POINT ( 'NONE',  ( 32.09707732552327286, 88.32801317409231956, -3.000000000000000000 ) ) ;
#3884 = CARTESIAN_POINT ( 'NONE',  ( 19.27821517812503060, 62.76906990284727783, 3.078125000614517326 ) ) ;
#3885 = VECTOR ( 'NONE', #1664, 1000.000000000000000 ) ;
#3886 = FACE_OUTER_BOUND ( 'NONE', #9493, .T. ) ;
#3887 = ORIENTED_EDGE ( 'NONE', *, *, #8474, .F. ) ;
#3888 = VECTOR ( 'NONE', #4836, 1000.000000000000114 ) ;
#3889 = CARTESIAN_POINT ( 'NONE',  ( 3.800000000000015365, 108.0133283987163111, 4.962499999999999467 ) ) ;
#3890 = ADVANCED_FACE ( 'NONE', ( #6629 ), #12464, .F. ) ;
#3891 = DIRECTION ( 'NONE',  ( -0.000000000000000000, -0.000000000000000000, -1.000000000000000000 ) ) ;
#3892 = CARTESIAN_POINT ( 'NONE',  ( 18.35999867260799689, 66.24638416932324958, -1.000000000000000000 ) ) ;
#3893 = ORIENTED_EDGE ( 'NONE', *, *, #11837, .F. ) ;
#3894 = FACE_OUTER_BOUND ( 'NONE', #3397, .T. ) ;
#3895 = EDGE_CURVE ( 'NONE', #6695, #11510, #4481, .T. ) ;
#3896 = ORIENTED_EDGE ( 'NONE', *, *, #1271, .F. ) ;
#3897 = LINE ( 'NONE', #4932, #2112 ) ;
#3898 = CARTESIAN_POINT ( 'NONE',  ( 50.72178482187501203, 62.76906990284730625, 3.659375000614517592 ) ) ;
#3899 = EDGE_LOOP ( 'NONE', ( #11490, #5187, #478, #8574 ) ) ;
#3900 = CARTESIAN_POINT ( 'NONE',  ( 66.19999999999998863, 90.00000000000000000, 4.774999999999999467 ) ) ;
#3901 = CARTESIAN_POINT ( 'NONE',  ( -2.179634403564815859, -5.614030811971695734, 0.000000000000000000 ) ) ;
#3902 = EDGE_LOOP ( 'NONE', ( #3289, #9942, #2249, #1190 ) ) ;
#3903 = FACE_OUTER_BOUND ( 'NONE', #2446, .T. ) ;
#3904 = EDGE_CURVE ( 'NONE', #4989, #8980, #10370, .T. ) ;
#3905 = FACE_OUTER_BOUND ( 'NONE', #3336, .T. ) ;
#3906 = AXIS2_PLACEMENT_3D ( 'NONE', #2525, #3510, #2394 ) ;
#3907 = DIRECTION ( 'NONE',  ( 0.000000000000000000, 0.000000000000000000, 1.000000000000000000 ) ) ;
#3908 = DIRECTION ( 'NONE',  ( -1.000000000000000000, 0.000000000000000000, 0.000000000000000000 ) ) ;
#3909 = CARTESIAN_POINT ( 'NONE',  ( 50.72178482187499071, 117.2309300971526937, 3.809375000614517504 ) ) ;
#3910 = ORIENTED_EDGE ( 'NONE', *, *, #2223, .F. ) ;
#3911 =( BOUNDED_CURVE ( )  B_SPLINE_CURVE ( 2, ( #11089, #90, #6253, #9198, #2211, #6188, #2141 ),
 .UNSPECIFIED., .F., .F. ) 
 B_SPLINE_CURVE_WITH_KNOTS ( ( 3, 2, 2, 3 ),
 ( 0.1999999999999999833, 0.2333333333333333925, 0.2666666666666668295, 0.3000000000000002109 ),
 .UNSPECIFIED. ) 
 CURVE ( )  GEOMETRIC_REPRESENTATION_ITEM ( )  RATIONAL_B_SPLINE_CURVE ( ( 1.000000000000000222, 0.8660254037844385966, 1.000000000000000000, 0.8660254037844387076, 1.000000000000000000, 0.8660254037844378194, 1.000000000000000888 ) ) 
 REPRESENTATION_ITEM ( '' )  );
#3912 = DIRECTION ( 'NONE',  ( 0.000000000000000000, 1.000000000000000000, 0.000000000000000000 ) ) ;
#3913 = EDGE_LOOP ( 'NONE', ( #974, #10572, #11415, #10187 ) ) ;
#3914 = AXIS2_PLACEMENT_3D ( 'NONE', #688, #9538, #4698 ) ;
#3915 = DIRECTION ( 'NONE',  ( 0.4719909656437442647, -0.8816033849473842166, 2.775557561595757269E-17 ) ) ;
#3916 = LINE ( 'NONE', #8936, #3319 ) ;
#3917 = DIRECTION ( 'NONE',  ( 1.000000000000000000, 0.000000000000000000, 5.337610695313252124E-17 ) ) ;
#3918 = ADVANCED_FACE ( 'NONE', ( #9646 ), #5654, .T. ) ;
#3919 = DIRECTION ( 'NONE',  ( 0.000000000000000000, 0.000000000000000000, 1.000000000000000000 ) ) ;
#3920 = DIRECTION ( 'NONE',  ( 0.000000000000000000, 0.000000000000000000, 1.000000000000000000 ) ) ;
#3921 = ORIENTED_EDGE ( 'NONE', *, *, #1393, .T. ) ;
#3922 = LINE ( 'NONE', #7046, #7424 ) ;
#3923 = CARTESIAN_POINT ( 'NONE',  ( 35.00000000000000000, 90.00000000000000000, -18.00000000000000355 ) ) ;
#3924 = ORIENTED_EDGE ( 'NONE', *, *, #462, .T. ) ;
#3925 = EDGE_CURVE ( 'NONE', #11880, #5406, #11834, .T. ) ;
#3926 = FILL_AREA_STYLE ('',( #7775 ) ) ;
#3927 = VERTEX_POINT ( 'NONE', #5387 ) ;
#3928 =( NAMED_UNIT ( * ) SI_UNIT ( $, .STERADIAN. ) SOLID_ANGLE_UNIT ( ) );
#3929 = ORIENTED_EDGE ( 'NONE', *, *, #6752, .F. ) ;
#3930 = ADVANCED_FACE ( 'NONE', ( #6374 ), #7457, .T. ) ;
#3931 = EDGE_CURVE ( 'NONE', #451, #12353, #798, .T. ) ;
#3932 = CARTESIAN_POINT ( 'NONE',  ( 1.649999999999999911, 3.490243377569956061E-16, -2.849999999999999645 ) ) ;
#3933 = CARTESIAN_POINT ( 'NONE',  ( 3.800000000000015365, 90.00000000000000000, 3.312500001229034652 ) ) ;
#3934 = AXIS2_PLACEMENT_3D ( 'NONE', #7413, #6423, #9506 ) ;
#3935 = VERTEX_POINT ( 'NONE', #1468 ) ;
#3936 = DIRECTION ( 'NONE',  ( 1.000000000000000000, 0.000000000000000000, 0.000000000000000000 ) ) ;
#3937 = ORIENTED_EDGE ( 'NONE', *, *, #1799, .F. ) ;
#3938 = CARTESIAN_POINT ( 'NONE',  ( -36.66666666666665009, 46.12451549659709116, 7.999999999999996447 ) ) ;
#3939 = ORIENTED_EDGE ( 'NONE', *, *, #12047, .F. ) ;
#3940 = FACE_OUTER_BOUND ( 'NONE', #846, .T. ) ;
#3941 = AXIS2_PLACEMENT_3D ( 'NONE', #1817, #7963, #5073 ) ;
#3942 = EDGE_LOOP ( 'NONE', ( #1502, #10128, #4621, #3058, #6530, #6932 ) ) ;
#3943 = AXIS2_PLACEMENT_3D ( 'NONE', #5939, #9938, #6203 ) ;
#3944 = CARTESIAN_POINT ( 'NONE',  ( 35.00000000000000000, 90.00000000000000000, 4.000000000000000000 ) ) ;
#3945 = CARTESIAN_POINT ( 'NONE',  ( 35.00000000000000000, 126.0266567974326222, 3.087499999999999911 ) ) ;
#3946 = CARTESIAN_POINT ( 'NONE',  ( -6.666666666666660745, 2.000000000000000000, -1.599999999999992539 ) ) ;
#3947 = CARTESIAN_POINT ( 'NONE',  ( 35.00000000000000000, 126.3079067962035822, 4.240625000614517859 ) ) ;
#3948 = CARTESIAN_POINT ( 'NONE',  ( 50.00000000000000000, 121.2009999999999934, 1.500000000000001332 ) ) ;
#3949 = EDGE_CURVE ( 'NONE', #4463, #4318, #12470, .T. ) ;
#3950 = CIRCLE ( 'NONE', #1218, 29.99999999999999645 ) ;
#3951 = EDGE_LOOP ( 'NONE', ( #7018, #6032, #5943, #8314 ) ) ;
#3952 = DIRECTION ( 'NONE',  ( -0.000000000000000000, 0.000000000000000000, -1.000000000000000000 ) ) ;
#3953 = CARTESIAN_POINT ( 'NONE',  ( 52.49999999999996447, 90.00000000000000000, -10.00000000000000000 ) ) ;
#3954 = CARTESIAN_POINT ( 'NONE',  ( 0.000000000000000000, -0.5773502691896253980, 1.000000000000000000 ) ) ;
#3955 = EDGE_LOOP ( 'NONE', ( #6679, #6593 ) ) ;
#3956 = CARTESIAN_POINT ( 'NONE',  ( 9.999999999999994671, 70.41451884327426569, -3.000000000000000000 ) ) ;
#3957 = VERTEX_POINT ( 'NONE', #10568 ) ;
#3958 = LINE ( 'NONE', #1058, #6070 ) ;
#3959 = PLANE ( 'NONE',  #3072 ) ;
#3960 = ORIENTED_EDGE ( 'NONE', *, *, #9679, .T. ) ;
#3961 = AXIS2_PLACEMENT_3D ( 'NONE', #10136, #7132, #1371 ) ;
#3962 = CARTESIAN_POINT ( 'NONE',  ( 66.44356964374999563, 71.84604660189820891, 3.246875000614517059 ) ) ;
#3963 = EDGE_CURVE ( 'NONE', #1810, #10261, #9517, .T. ) ;
#3964 = CARTESIAN_POINT ( 'NONE',  ( 40.00000000000000000, 90.00000000000000000, -5.000000000000000000 ) ) ;
#3965 = EDGE_CURVE ( 'NONE', #8608, #3811, #406, .T. ) ;
#3966 = VECTOR ( 'NONE', #9497, 1000.000000000000000 ) ;
#3967 = CARTESIAN_POINT ( 'NONE',  ( 35.00000000000000000, 90.00000000000000000, 22.38477631085024555 ) ) ;
#3968 = CARTESIAN_POINT ( 'NONE',  ( 25.83484861008832567, 94.00000000000000000, -10.00000000000000000 ) ) ;
#3969 = VECTOR ( 'NONE', #3787, 1000.000000000000000 ) ;
#3970 = CARTESIAN_POINT ( 'NONE',  ( -65.00000000000004263, 38.66025403784436065, 3.000000000000000000 ) ) ;
#3971 = DIRECTION ( 'NONE',  ( -0.8660254037844394848, -0.4999999999999984457, -0.000000000000000000 ) ) ;
#3972 = LINE ( 'NONE', #7823, #7240 ) ;
#3973 = ORIENTED_EDGE ( 'NONE', *, *, #4201, .F. ) ;
#3974 = AXIS2_PLACEMENT_3D ( 'NONE', #3745, #10730, #1774 ) ;
#3975 = DIRECTION ( 'NONE',  ( 0.000000000000000000, 0.000000000000000000, 1.000000000000000000 ) ) ;
#3976 = ORIENTED_EDGE ( 'NONE', *, *, #12676, .F. ) ;
#3977 = ADVANCED_FACE ( 'NONE', ( #8410 ), #6821, .F. ) ;
#3978 = DIRECTION ( 'NONE',  ( 0.000000000000000000, 1.000000000000000000, 0.000000000000000000 ) ) ;
#3979 = CARTESIAN_POINT ( 'NONE',  ( 50.59999999999999432, 117.0199925980744666, 3.500000000000000444 ) ) ;
#3980 = CARTESIAN_POINT ( 'NONE',  ( -60.00000000000000000, 30.00000000000000000, 1.000000000000001776 ) ) ;
#3981 = DIRECTION ( 'NONE',  ( -0.000000000000000000, 1.000000000000000000, -0.000000000000000000 ) ) ;
#3982 = AXIS2_PLACEMENT_3D ( 'NONE', #1402, #12333, #10298 ) ;
#3983 = ORIENTED_EDGE ( 'NONE', *, *, #4725, .F. ) ;
#3984 = CYLINDRICAL_SURFACE ( 'NONE', #6794, 1.500000000000000222 ) ;
#3985 = DIRECTION ( 'NONE',  ( -1.000000000000000000, 0.000000000000000000, 0.000000000000000000 ) ) ;
#3986 = ORIENTED_EDGE ( 'NONE', *, *, #1729, .F. ) ;
#3987 = SURFACE_STYLE_USAGE ( .BOTH. , #100 ) ;
#3988 = DIRECTION ( 'NONE',  ( 0.000000000000000000, 0.000000000000000000, 1.000000000000000000 ) ) ;
#3989 = VERTEX_POINT ( 'NONE', #6501 ) ;
#3990 =( NAMED_UNIT ( * ) SI_UNIT ( $, .STERADIAN. ) SOLID_ANGLE_UNIT ( ) );
#3991 = VERTEX_POINT ( 'NONE', #8477 ) ;
#3992 = EDGE_CURVE ( 'NONE', #11985, #3143, #10495, .T. ) ;
#3993 = CARTESIAN_POINT ( 'NONE',  ( 3.591865698314129496, 91.49237114305354623, 2.999999999999999556 ) ) ;
#3994 = AXIS2_PLACEMENT_3D ( 'NONE', #3703, #8665, #7617 ) ;
#3995 = DIRECTION ( 'NONE',  ( 1.000000000000000000, 0.000000000000000000, -0.000000000000000000 ) ) ;
#3996 = ORIENTED_EDGE ( 'NONE', *, *, #7915, .F. ) ;
#3997 = ORIENTED_EDGE ( 'NONE', *, *, #4300, .T. ) ;
#3998 = DIRECTION ( 'NONE',  ( -1.000000000000000000, 0.000000000000000000, 0.000000000000000000 ) ) ;
#3999 = ORIENTED_EDGE ( 'NONE', *, *, #1331, .F. ) ;
#4000 = ADVANCED_FACE ( 'NONE', ( #8544 ), #5150, .F. ) ;
#4001 = DIRECTION ( 'NONE',  ( -0.000000000000000000, 0.000000000000000000, -1.000000000000000000 ) ) ;
#4002 = EDGE_CURVE ( 'NONE', #10475, #8376, #3574, .T. ) ;
#4003 = ORIENTED_EDGE ( 'NONE', *, *, #2916, .T. ) ;
#4004 = VECTOR ( 'NONE', #5626, 1000.000000000000000 ) ;
#4005 = FACE_OUTER_BOUND ( 'NONE', #8761, .T. ) ;
#4006 = VERTEX_POINT ( 'NONE', #6435 ) ;
#4007 = DIRECTION ( 'NONE',  ( -1.000000000000000000, -0.000000000000000000, -0.000000000000000000 ) ) ;
#4008 = CARTESIAN_POINT ( 'NONE',  ( 50.72178482187501203, 62.76906990284730625, 4.503125000614517148 ) ) ;
#4009 = DIRECTION ( 'NONE',  ( -0.000000000000000000, -0.000000000000000000, -1.000000000000000000 ) ) ;
#4010 = CARTESIAN_POINT ( 'NONE',  ( 3.800000000000015365, 90.00000000000000000, 2.862500001229034474 ) ) ;
#4011 = B_SPLINE_CURVE_WITH_KNOTS ( 'NONE', 3,
 ( #1477, #11486, #3583, #5662 ),
 .UNSPECIFIED., .F., .F.,
 ( 4, 4 ),
 ( 0.000000000000000000, 0.5999999999999994227 ),
 .UNSPECIFIED. ) ;
#4012 = EDGE_CURVE ( 'NONE', #8585, #6517, #10433, .T. ) ;
#4013 = AXIS2_PLACEMENT_3D ( 'NONE', #1225, #5456, #12158 ) ;
#4014 = DIRECTION ( 'NONE',  ( 5.337610695313252124E-17, 0.000000000000000000, -1.000000000000000000 ) ) ;
#4015 = ORIENTED_EDGE ( 'NONE', *, *, #4317, .F. ) ;
#4016 = LINE ( 'NONE', #4799, #3666 ) ;
#4017 = DIRECTION ( 'NONE',  ( -0.5000000000000042188, 0.000000000000000000, 0.8660254037844361541 ) ) ;
#4018 = CARTESIAN_POINT ( 'NONE',  ( 43.37907491812715932, 120.1818777491212700, 3.000000000000001332 ) ) ;
#4019 = VERTEX_POINT ( 'NONE', #7944 ) ;
#4020 = DIRECTION ( 'NONE',  ( -0.000000000000000000, -0.000000000000000000, -1.000000000000000000 ) ) ;
#4021 = ORIENTED_EDGE ( 'NONE', *, *, #9946, .T. ) ;
#4022 = LINE ( 'NONE', #7086, #4826 ) ;
#4023 = CARTESIAN_POINT ( 'NONE',  ( 66.44356964374999563, 90.00000000000000000, 4.578125000614516438 ) ) ;
#4024 = ADVANCED_FACE ( 'NONE', ( #8920 ), #3959, .T. ) ;
#4025 = VERTEX_POINT ( 'NONE', #10817 ) ;
#4026 = CARTESIAN_POINT ( 'NONE',  ( 66.44356964374999563, 90.00000000000000000, 4.184375000614516615 ) ) ;
#4027 = DIRECTION ( 'NONE',  ( -1.000000000000000000, -0.000000000000000000, -0.000000000000000000 ) ) ;
#4028 = VECTOR ( 'NONE', #5349, 1000.000000000000227 ) ;
#4029 = DIRECTION ( 'NONE',  ( -1.000000000000000000, 0.000000000000000000, 0.000000000000000000 ) ) ;
#4030 = LINE ( 'NONE', #9906, #10326 ) ;
#4031 = CARTESIAN_POINT ( 'NONE',  ( 35.00000000000000000, 90.00000000000000000, -8.000000000000000000 ) ) ;
#4032 = CARTESIAN_POINT ( 'NONE',  ( 6.499999999999999112, 79.07477288111861924, 0.9999999999999997780 ) ) ;
#4033 = CARTESIAN_POINT ( 'NONE',  ( 5.000000000000004441, 76.58915998087155685, 2.500000000000000444 ) ) ;
#4034 = ADVANCED_FACE ( 'NONE', ( #4678 ), #2149, .F. ) ;
#4035 = ORIENTED_EDGE ( 'NONE', *, *, #3494, .F. ) ;
#4036 = CIRCLE ( 'NONE', #6104, 3.500000000000003109 ) ;
#4037 = CARTESIAN_POINT ( 'NONE',  ( 35.49999999999995026, 119.0000000000000000, -1.000000000000000000 ) ) ;
#4038 = EDGE_LOOP ( 'NONE', ( #12074, #5887, #12813, #3395 ) ) ;
#4039 = PRESENTATION_STYLE_ASSIGNMENT (( #6052 ) ) ;
#4040 = FACE_OUTER_BOUND ( 'NONE', #3217, .T. ) ;
#4041 = CARTESIAN_POINT ( 'NONE',  ( 20.00000000000000355, 0.000000000000000000, 10.00000000000000000 ) ) ;
#4042 = CARTESIAN_POINT ( 'NONE',  ( 1.436050757534458100, -5.516136167806656943, -0.8000000000000000444 ) ) ;
#4043 = MECHANICAL_DESIGN_GEOMETRIC_PRESENTATION_REPRESENTATION (  '', ( #8836 ), #11760 ) ;
#4044 = ORIENTED_EDGE ( 'NONE', *, *, #987, .T. ) ;
#4045 = FACE_OUTER_BOUND ( 'NONE', #7966, .T. ) ;
#4046 = EDGE_CURVE ( 'NONE', #4989, #681, #7284, .T. ) ;
#4047 = VERTEX_POINT ( 'NONE', #5053 ) ;
#4048 = CIRCLE ( 'NONE', #4457, 1.599999999999997202 ) ;
#4049 = DIRECTION ( 'NONE',  ( 0.000000000000000000, 0.5150380737757249694, 0.8571673013836860200 ) ) ;
#4050 = EDGE_CURVE ( 'NONE', #408, #2666, #70, .T. ) ;
#4051 = EDGE_LOOP ( 'NONE', ( #5358, #3887, #3728, #5402 ) ) ;
#4052 = DIRECTION ( 'NONE',  ( -1.000000000000000000, 0.000000000000000000, 0.000000000000000000 ) ) ;
#4053 = VERTEX_POINT ( 'NONE', #7150 ) ;
#4054 = CARTESIAN_POINT ( 'NONE',  ( 3.800000000000015365, 90.00000000000000000, 4.100000000000000533 ) ) ;
#4055 = CARTESIAN_POINT ( 'NONE',  ( 35.00000000000000000, 90.00000000000000000, -5.000000000000000000 ) ) ;
#4056 = VERTEX_POINT ( 'NONE', #2189 ) ;
#4057 = AXIS2_PLACEMENT_3D ( 'NONE', #6383, #5075, #93 ) ;
#4058 = ORIENTED_EDGE ( 'NONE', *, *, #7681, .F. ) ;
#4059 = DIRECTION ( 'NONE',  ( 0.000000000000000000, 0.000000000000000000, 1.000000000000000000 ) ) ;
#4060 = ORIENTED_EDGE ( 'NONE', *, *, #9131, .T. ) ;
#4061 = CARTESIAN_POINT ( 'NONE',  ( 19.27821517812500574, 117.2309300971526937, 4.278125000614516615 ) ) ;
#4062 = EDGE_CURVE ( 'NONE', #11890, #1701, #8334, .T. ) ;
#4063 =( GEOMETRIC_REPRESENTATION_CONTEXT ( 3 ) GLOBAL_UNCERTAINTY_ASSIGNED_CONTEXT ( ( #11132 ) ) GLOBAL_UNIT_ASSIGNED_CONTEXT ( ( #10316, #8424, #9400 ) ) REPRESENTATION_CONTEXT ( 'NONE', 'WORKASPACE' ) );
#4064 = ORIENTED_EDGE ( 'NONE', *, *, #707, .F. ) ;
#4065 = DIRECTION ( 'NONE',  ( -1.000000000000000000, -0.000000000000000000, -0.000000000000000000 ) ) ;
#4066 = ORIENTED_EDGE ( 'NONE', *, *, #2241, .T. ) ;
#4067 = EDGE_CURVE ( 'NONE', #1627, #4019, #10483, .T. ) ;
#4068 = LINE ( 'NONE', #7860, #7552 ) ;
#4069 = CIRCLE ( 'NONE', #3856, 29.99999999999999645 ) ;
#4070 = CARTESIAN_POINT ( 'NONE',  ( 35.00000000000000000, 126.3079067962036106, 4.240625000614517859 ) ) ;
#4071 = MECHANICAL_DESIGN_GEOMETRIC_PRESENTATION_REPRESENTATION (  '', ( #9491 ), #493 ) ;
#4072 = CARTESIAN_POINT ( 'NONE',  ( 0.000000000000000000, 1.154700538379252350, 7.017607234860990640E-28 ) ) ;
#4073 = CARTESIAN_POINT ( 'NONE',  ( 3.800000000000015365, 108.0133283987163111, 2.825000001229034385 ) ) ;
#4074 = EDGE_CURVE ( 'NONE', #2347, #11985, #7410, .T. ) ;
#4075 = CARTESIAN_POINT ( 'NONE',  ( 3.800000000000055334, 71.98667160128364628, 4.137500000000000178 ) ) ;
#4076 = VERTEX_POINT ( 'NONE', #2512 ) ;
#4077 = CARTESIAN_POINT ( 'NONE',  ( 19.40000000000002700, 62.98000740192551206, 3.725000000000000089 ) ) ;
#4078 = VECTOR ( 'NONE', #1019, 1000.000000000000000 ) ;
#4079 = DIRECTION ( 'NONE',  ( 1.000000000000000000, 0.000000000000000000, -0.000000000000000000 ) ) ;
#4080 = CARTESIAN_POINT ( 'NONE',  ( 54.68276421697586187, 114.3044457306839234, 3.000000000000001332 ) ) ;
#4081 = EDGE_LOOP ( 'NONE', ( #3032, #2475, #758, #4775 ) ) ;
#4082 = CONICAL_SURFACE ( 'NONE', #502, 1.500000000000001332, 1.029744260000000411 ) ;
#4083 = DIRECTION ( 'NONE',  ( 0.5000000000000045519, -0.8660254037844360431, 0.000000000000000000 ) ) ;
#4084 = EDGE_LOOP ( 'NONE', ( #2156, #12544, #8259, #12865, #7300 ) ) ;
#4085 = DIRECTION ( 'NONE',  ( 0.000000000000000000, 1.000000000000000000, 0.000000000000000000 ) ) ;
#4086 = CARTESIAN_POINT ( 'NONE',  ( 50.72178482187501203, 62.76906990284730625, 3.153125000614517504 ) ) ;
#4087 = ORIENTED_EDGE ( 'NONE', *, *, #8637, .F. ) ;
#4088 = CARTESIAN_POINT ( 'NONE',  ( 19.27821517812500574, 117.2309300971526937, 2.984375000614517326 ) ) ;
#4089 = DIRECTION ( 'NONE',  ( 0.000000000000000000, 0.000000000000000000, 1.000000000000000000 ) ) ;
#4090 = AXIS2_PLACEMENT_3D ( 'NONE', #6512, #6448, #6576 ) ;
#4091 = EDGE_CURVE ( 'NONE', #10444, #9939, #4535, .T. ) ;
#4092 = FACE_OUTER_BOUND ( 'NONE', #1678, .T. ) ;
#4093 = EDGE_CURVE ( 'NONE', #12605, #11420, #6845, .T. ) ;
#4094 = CIRCLE ( 'NONE', #8680, 2.396199811936269963 ) ;
#4095 = CARTESIAN_POINT ( 'NONE',  ( 0.000000000000000000, 0.000000000000000000, -3.000000000000000000 ) ) ;
#4096 = CARTESIAN_POINT ( 'NONE',  ( 33.90709641728108892, 93.16671150547063007, 4.800000000000000711 ) ) ;
#4097 =( REPRESENTATION_RELATIONSHIP ('NONE','NONE', #1997, #1066 ) REPRESENTATION_RELATIONSHIP_WITH_TRANSFORMATION ( #1431 )SHAPE_REPRESENTATION_RELATIONSHIP( ) );
#4098 = AXIS2_PLACEMENT_3D ( 'NONE', #9382, #2654, #11473 ) ;
#4099 = PLANE ( 'NONE',  #3050 ) ;
#4100 = LINE ( 'NONE', #10951, #12336 ) ;
#4101 = CARTESIAN_POINT ( 'NONE',  ( 1.040000000000000036, -1.154700538379251240, 1.014316938424154191E-17 ) ) ;
#4102 = ORIENTED_EDGE ( 'NONE', *, *, #7335, .F. ) ;
#4103 = DIRECTION ( 'NONE',  ( -0.000000000000000000, 1.000000000000000000, -0.000000000000000000 ) ) ;
#4104 = VERTEX_POINT ( 'NONE', #12517 ) ;
#4105 = CARTESIAN_POINT ( 'NONE',  ( 66.19999999999998863, 90.00000000000000000, 3.425000000000000266 ) ) ;
#4106 = CARTESIAN_POINT ( 'NONE',  ( 35.00000000000000000, 90.00000000000000000, 5.000000000000000000 ) ) ;
#4107 = ADVANCED_FACE ( 'NONE', ( #3561 ), #9435, .F. ) ;
#4108 = CARTESIAN_POINT ( 'NONE',  ( -0.1325741768533960641, -4.273461295629625845, -0.8000000000000000444 ) ) ;
#4109 = ORIENTED_EDGE ( 'NONE', *, *, #5242, .T. ) ;
#4110 = CARTESIAN_POINT ( 'NONE',  ( 4.999999999999962697, 79.07477288111861924, -3.000000000000000000 ) ) ;
#4111 = CARTESIAN_POINT ( 'NONE',  ( 3.800000000000015365, 90.00000000000000000, 3.650000000000000355 ) ) ;
#4112 = ORIENTED_EDGE ( 'NONE', *, *, #11318, .F. ) ;
#4113 = FILL_AREA_STYLE ('',( #161 ) ) ;
#4114 = ORIENTED_EDGE ( 'NONE', *, *, #8856, .T. ) ;
#4115 = CIRCLE ( 'NONE', #1389, 4.338286831716297698 ) ;
#4116 = CARTESIAN_POINT ( 'NONE',  ( 62.73514746974691292, 98.48596457872595522, 4.000000000000000000 ) ) ;
#4117 = ORIENTED_EDGE ( 'NONE', *, *, #8525, .F. ) ;
#4118 = CYLINDRICAL_SURFACE ( 'NONE', #6528, 30.00000000000000000 ) ;
#4119 = DIRECTION ( 'NONE',  ( -0.000000000000000000, 0.000000000000000000, -1.000000000000000000 ) ) ;
#4120 = EDGE_CURVE ( 'NONE', #5822, #6093, #11330, .T. ) ;
#4121 = EDGE_LOOP ( 'NONE', ( #563, #12287, #11521, #3896 ) ) ;
#4122 = EDGE_CURVE ( 'NONE', #7384, #1569, #11528, .T. ) ;
#4123 = EDGE_CURVE ( 'NONE', #4591, #9403, #333, .T. ) ;
#4124 = EDGE_LOOP ( 'NONE', ( #3351, #6950, #8065, #5022 ) ) ;
#4125 = VECTOR ( 'NONE', #3751, 1000.000000000000000 ) ;
#4126 = PLANE ( 'NONE',  #11392 ) ;
#4127 = ORIENTED_EDGE ( 'NONE', *, *, #12932, .T. ) ;
#4128 = PRODUCT_CONTEXT ( 'NONE', #7514, 'mechanical' ) ;
#4129 = CARTESIAN_POINT ( 'NONE',  ( 19.27821517812500574, 117.2309300971526937, 3.378125000614517148 ) ) ;
#4130 = VERTEX_POINT ( 'NONE', #10420 ) ;
#4131 = FACE_BOUND ( 'NONE', #5458, .T. ) ;
#4132 = DIRECTION ( 'NONE',  ( 0.5000000000000038858, -0.8660254037844362651, 0.000000000000000000 ) ) ;
#4133 = ORIENTED_EDGE ( 'NONE', *, *, #9196, .F. ) ;
#4134 = CARTESIAN_POINT ( 'NONE',  ( 35.00000000000000000, 90.00000000000000000, 6.000000000000000000 ) ) ;
#4135 = DIRECTION ( 'NONE',  ( 0.000000000000000000, 0.000000000000000000, -1.000000000000000000 ) ) ;
#4136 = AXIS2_PLACEMENT_3D ( 'NONE', #7557, #8609, #9648 ) ;
#4137 = CARTESIAN_POINT ( 'NONE',  ( 6.626776019045580668, 99.74475042915889844, 1.000000000000003109 ) ) ;
#4138 = CARTESIAN_POINT ( 'NONE',  ( 66.19999999999997442, 108.0133283987163253, 3.125000001229034208 ) ) ;
#4139 = ADVANCED_FACE ( 'NONE', ( #10553 ), #9309, .F. ) ;
#4140 = CARTESIAN_POINT ( 'NONE',  ( 12.66025403784434822, 85.80682368868758658, -1.000000000000000000 ) ) ;
#4141 = ORIENTED_EDGE ( 'NONE', *, *, #11691, .F. ) ;
#4142 = CARTESIAN_POINT ( 'NONE',  ( 19.40000000000002700, 62.98000740192551206, 4.174999999999999822 ) ) ;
#4143 = CYLINDRICAL_SURFACE ( 'NONE', #7929, 1.599999999999993872 ) ;
#4144 = CARTESIAN_POINT ( 'NONE',  ( 0.000000000000000000, 0.000000000000000000, -1.000000000000000000 ) ) ;
#4145 = CIRCLE ( 'NONE', #11251, 1.599999999999986766 ) ;
#4146 = ORIENTED_EDGE ( 'NONE', *, *, #2335, .T. ) ;
#4147 = DIRECTION ( 'NONE',  ( -0.000000000000000000, 1.000000000000000000, -0.000000000000000000 ) ) ;
#4148 = VERTEX_POINT ( 'NONE', #6360 ) ;
#4149 = CYLINDRICAL_SURFACE ( 'NONE', #10258, 4.000000000000000000 ) ;
#4150 = CARTESIAN_POINT ( 'NONE',  ( 31.72849223410691266, 88.75612020769642641, 6.000000000000000000 ) ) ;
#4151 = ORIENTED_EDGE ( 'NONE', *, *, #8018, .T. ) ;
#4152 = CARTESIAN_POINT ( 'NONE',  ( 35.00000000000000711, 53.69209320379640360, 3.621875000614517059 ) ) ;
#4153 = CARTESIAN_POINT ( 'NONE',  ( -60.00000000000000000, 30.00000000000000000, -3.000000000000000000 ) ) ;
#4154 = EDGE_CURVE ( 'NONE', #6792, #8177, #10375, .T. ) ;
#4156 = VECTOR ( 'NONE', #1768, 1000.000000000000227 ) ;
#4155 = CARTESIAN_POINT ( 'NONE',  ( 35.00000000000000000, 90.00000000000000000, 6.000000000000000000 ) ) ;
#4157 = DIRECTION ( 'NONE',  ( 0.000000000000000000, 0.000000000000000000, -1.000000000000000000 ) ) ;
#4158 = DIRECTION ( 'NONE',  ( 0.000000000000000000, -1.000000000000000000, 0.000000000000000000 ) ) ;
#4159 = CARTESIAN_POINT ( 'NONE',  ( -63.99999999999998579, 36.92820323027551410, 2.500000000000000000 ) ) ;
#4160 = LINE ( 'NONE', #11280, #9932 ) ;
#4161 = EDGE_CURVE ( 'NONE', #12628, #11494, #3702, .T. ) ;
#4162 = VECTOR ( 'NONE', #6493, 1000.000000000000000 ) ;
#4163 = EDGE_CURVE ( 'NONE', #1698, #4578, #12048, .T. ) ;
#4164 = CARTESIAN_POINT ( 'NONE',  ( 1.040000000000000036, 0.000000000000000000, -1.000000000000000000 ) ) ;
#4165 = DIRECTION ( 'NONE',  ( -0.8090169943749457859, -0.5877852522924753575, 0.000000000000000000 ) ) ;
#4166 = EDGE_LOOP ( 'NONE', ( #9813, #8577, #3011, #10516 ) ) ;
#4167 = CARTESIAN_POINT ( 'NONE',  ( 4.999999999999962697, 79.07477288111861924, -1.000000000000000000 ) ) ;
#4168 = ORIENTED_EDGE ( 'NONE', *, *, #10496, .T. ) ;
#4169 =( NAMED_UNIT ( * ) SI_UNIT ( $, .STERADIAN. ) SOLID_ANGLE_UNIT ( ) );
#4170 = VECTOR ( 'NONE', #4673, 1000.000000000000000 ) ;
#4171 = CIRCLE ( 'NONE', #12530, 28.99999999999999289 ) ;
#4172 = CYLINDRICAL_SURFACE ( 'NONE', #3237, 1.500000000000002665 ) ;
#4173 = CARTESIAN_POINT ( 'NONE',  ( 1.000000000000000000, -4.873461295629625489, -0.8000000000000000444 ) ) ;
#4174 = APPLICATION_CONTEXT ( 'automotive_design' ) ;
#4175 = DIRECTION ( 'NONE',  ( 0.000000000000000000, 0.000000000000000000, -1.000000000000000000 ) ) ;
#4176 = EDGE_LOOP ( 'NONE', ( #7446, #10998, #5054, #11861, #746 ) ) ;
#4177 = LINE ( 'NONE', #9268, #9301 ) ;
#4178 = DIRECTION ( 'NONE',  ( 0.000000000000000000, 0.000000000000000000, 1.000000000000000000 ) ) ;
#4179 = ORIENTED_EDGE ( 'NONE', *, *, #10241, .F. ) ;
#4180 = AXIS2_PLACEMENT_3D ( 'NONE', #12183, #2375, #8067 ) ;
#4181 = EDGE_LOOP ( 'NONE', ( #8232, #6734, #4573, #3734 ) ) ;
#4182 = CYLINDRICAL_SURFACE ( 'NONE', #12783, 1.499999999999998668 ) ;
#4183 = VERTEX_POINT ( 'NONE', #3496 ) ;
#4184 = EDGE_CURVE ( 'NONE', #10254, #8585, #1587, .T. ) ;
#4185 = DIRECTION ( 'NONE',  ( 0.000000000000000000, 0.000000000000000000, -1.000000000000000000 ) ) ;
#4186 = CARTESIAN_POINT ( 'NONE',  ( 35.00000000000000000, 90.00000000000000000, 6.000000000000000000 ) ) ;
#4187 = ORIENTED_EDGE ( 'NONE', *, *, #2129, .F. ) ;
#4188 = VECTOR ( 'NONE', #12085, 1000.000000000000114 ) ;
#4189 = ORIENTED_EDGE ( 'NONE', *, *, #12070, .T. ) ;
#4190 = DIRECTION ( 'NONE',  ( -1.000000000000000000, 0.000000000000000000, -0.000000000000000000 ) ) ;
#4191 = ORIENTED_EDGE ( 'NONE', *, *, #8194, .F. ) ;
#4192 = PRODUCT_CONTEXT ( 'NONE', #11522, 'mechanical' ) ;
#4193 = CARTESIAN_POINT ( 'NONE',  ( 35.00000000000000000, 126.0266567974326222, 4.550000001229034474 ) ) ;
#4194 = VERTEX_POINT ( 'NONE', #9693 ) ;
#4195 = LINE ( 'NONE', #9026, #6963 ) ;
#4196 = PLANE ( 'NONE',  #9164 ) ;
#4197 = ORIENTED_EDGE ( 'NONE', *, *, #12920, .F. ) ;
#4198 = AXIS2_PLACEMENT_3D ( 'NONE', #11146, #3908, #2202 ) ;
#4199 = CYLINDRICAL_SURFACE ( 'NONE', #1280, 3.499999999999996003 ) ;
#4200 = CARTESIAN_POINT ( 'NONE',  ( 35.00000000000000000, 126.3079067962036106, 3.790625000614517237 ) ) ;
#4201 = EDGE_CURVE ( 'NONE', #10118, #2032, #760, .T. ) ;
#4202 = DIRECTION ( 'NONE',  ( 0.9347165045408830641, 0.3553942263724511608, 0.000000000000000000 ) ) ;
#4203 = DIRECTION ( 'NONE',  ( 0.000000000000000000, 0.000000000000000000, 1.000000000000000000 ) ) ;
#4204 = DIRECTION ( 'NONE',  ( 0.000000000000000000, -0.000000000000000000, 1.000000000000000000 ) ) ;
#4205 = ORIENTED_EDGE ( 'NONE', *, *, #3609, .F. ) ;
#4206 = CONICAL_SURFACE ( 'NONE', #11920, 1.500000000000001332, 1.029744260000000411 ) ;
#4207 = CARTESIAN_POINT ( 'NONE',  ( 50.59999999999999432, 117.0199925980744666, 3.950000000000000178 ) ) ;
#4208 = ORIENTED_EDGE ( 'NONE', *, *, #3432, .F. ) ;
#4209 = FACE_OUTER_BOUND ( 'NONE', #5639, .T. ) ;
#4210 = VERTEX_POINT ( 'NONE', #851 ) ;
#4211 = LINE ( 'NONE', #1189, #892 ) ;
#4212 = VERTEX_POINT ( 'NONE', #9823 ) ;
#4213 = EDGE_CURVE ( 'NONE', #2081, #12892, #10865, .T. ) ;
#4214 = CARTESIAN_POINT ( 'NONE',  ( 63.68224097532933570, 98.79369391286387270, 1.000000000000003109 ) ) ;
#4215 = PRODUCT_DEFINITION_CONTEXT ( 'detailed design', #2763, 'design' ) ;
#4216 = CARTESIAN_POINT ( 'NONE',  ( 35.00000000000000000, 126.3079067962035822, 3.790625000614517237 ) ) ;
#4218 = VERTEX_POINT ( 'NONE', #6617 ) ;
#4217 = EDGE_CURVE ( 'NONE', #11778, #4659, #912, .T. ) ;
#4219 = PLANE ( 'NONE',  #6313 ) ;
#4220 = AXIS2_PLACEMENT_3D ( 'NONE', #9224, #380, #247 ) ;
#4221 = CYLINDRICAL_SURFACE ( 'NONE', #8527, 28.99999999999999289 ) ;
#4222 = CARTESIAN_POINT ( 'NONE',  ( 35.00000000000000000, 90.00000000000000000, 5.000000000000000000 ) ) ;
#4223 = CARTESIAN_POINT ( 'NONE',  ( 3.800000000000004707, 90.00000000000000000, 6.000000000000000000 ) ) ;
#4224 = DIRECTION ( 'NONE',  ( 0.8660254037844361541, 0.5000000000000042188, 0.000000000000000000 ) ) ;
#4225 = CARTESIAN_POINT ( 'NONE',  ( -6.666666666666660745, -5.901290925839663970, 0.000000000000000000 ) ) ;
#4226 = AXIS2_PLACEMENT_3D ( 'NONE', #5936, #3004, #6986 ) ;
#4227 = CARTESIAN_POINT ( 'NONE',  ( 35.75000000000000711, 93.41869858279433458, 6.000000000000000000 ) ) ;
#4228 = EDGE_CURVE ( 'NONE', #11619, #12205, #4748, .T. ) ;
#4229 = CARTESIAN_POINT ( 'NONE',  ( 31.80092274341787828, 89.00581455129388075, 4.800000000000000711 ) ) ;
#4230 = CARTESIAN_POINT ( 'NONE',  ( 50.72178482187501203, 62.76906990284730625, 3.209375000614517415 ) ) ;
#4231 = EDGE_LOOP ( 'NONE', ( #2622, #11507 ) ) ;
#4232 = EDGE_CURVE ( 'NONE', #2543, #4549, #12710, .T. ) ;
#4233 = DIRECTION ( 'NONE',  ( 0.000000000000000000, 0.000000000000000000, -1.000000000000000000 ) ) ;
#4234 = ORIENTED_EDGE ( 'NONE', *, *, #11049, .F. ) ;
#4235 = CIRCLE ( 'NONE', #2563, 1.599999999999986766 ) ;
#4236 = EDGE_CURVE ( 'NONE', #4511, #10380, #770, .T. ) ;
#4237 = DIRECTION ( 'NONE',  ( 0.000000000000000000, 0.000000000000000000, 1.000000000000000000 ) ) ;
#4238 = FACE_OUTER_BOUND ( 'NONE', #4837, .T. ) ;
#4239 = DIRECTION ( 'NONE',  ( 0.5877852522924753575, -0.8090169943749457859, 0.000000000000000000 ) ) ;
#4240 = UNCERTAINTY_MEASURE_WITH_UNIT (LENGTH_MEASURE( 1.000000000000000082E-05 ), #9677, 'distance_accuracy_value', 'NONE');
#4241 = ORIENTED_EDGE ( 'NONE', *, *, #2794, .T. ) ;
#4242 = CARTESIAN_POINT ( 'NONE',  ( 34.50001850811341342, 118.9978265420697170, -1.000000000000000000 ) ) ;
#4243 = LINE ( 'NONE', #6258, #12121 ) ;
#4244 = VERTEX_POINT ( 'NONE', #12650 ) ;
#4245 = AXIS2_PLACEMENT_3D ( 'NONE', #12290, #2351, #7253 ) ;
#4246 = CARTESIAN_POINT ( 'NONE',  ( 0.1698013801012111523, -5.473461295629626022, -0.8000000000000000444 ) ) ;
#4247 = EDGE_LOOP ( 'NONE', ( #6545, #8623, #5310, #11924, #6213 ) ) ;
#4248 = ORIENTED_EDGE ( 'NONE', *, *, #10870, .T. ) ;
#4249 = LINE ( 'NONE', #8171, #5695 ) ;
#4250 = FACE_OUTER_BOUND ( 'NONE', #7438, .T. ) ;
#4251 = VERTEX_POINT ( 'NONE', #10617 ) ;
#4252 = EDGE_CURVE ( 'NONE', #1224, #4148, #970, .T. ) ;
#4253 = STYLED_ITEM ( 'NONE', ( #4039 ), #11356 ) ;
#4254 = EDGE_LOOP ( 'NONE', ( #7776, #8432, #10122, #3910 ) ) ;
#4255 = CARTESIAN_POINT ( 'NONE',  ( 33.50000000000000711, 79.80000000000001137, 8.000000000000000000 ) ) ;
#4256 = ORIENTED_EDGE ( 'NONE', *, *, #11576, .T. ) ;
#4257 = VECTOR ( 'NONE', #1450, 1000.000000000000000 ) ;
#4258 = APPLICATION_PROTOCOL_DEFINITION ( 'draft international standard', 'automotive_design', 1998, #6170 ) ;
#4259 = CARTESIAN_POINT ( 'NONE',  ( 50.72178482187501203, 62.76906990284730625, 3.153125000614517504 ) ) ;
#4260 = ORIENTED_EDGE ( 'NONE', *, *, #3451, .T. ) ;
#4261 = FACE_BOUND ( 'NONE', #6455, .T. ) ;
#4262 = LINE ( 'NONE', #9354, #6251 ) ;
#4263 = ORIENTED_EDGE ( 'NONE', *, *, #8751, .T. ) ;
#4264 = FACE_OUTER_BOUND ( 'NONE', #12945, .T. ) ;
#4265 = CARTESIAN_POINT ( 'NONE',  ( -60.00000000000000000, 30.00000000000000000, 9.999999999999996447 ) ) ;
#4266 = CARTESIAN_POINT ( 'NONE',  ( 19.40000000000000924, 117.0199925980744666, 3.687500001229034208 ) ) ;
#4267 = DIRECTION ( 'NONE',  ( 0.000000000000000000, -1.000000000000000000, 0.000000000000000000 ) ) ;
#4268 =( REPRESENTATION_RELATIONSHIP ('NONE','NONE', #1997, #4597 ) REPRESENTATION_RELATIONSHIP_WITH_TRANSFORMATION ( #12496 )SHAPE_REPRESENTATION_RELATIONSHIP( ) );
#4269 = DIRECTION ( 'NONE',  ( -0.000000000000000000, -0.000000000000000000, -1.000000000000000000 ) ) ;
#4270 = VERTEX_POINT ( 'NONE', #2899 ) ;
#4271 = CARTESIAN_POINT ( 'NONE',  ( 19.27821517812503060, 62.76906990284727783, 4.484375000614516438 ) ) ;
#4272 = ORIENTED_EDGE ( 'NONE', *, *, #7674, .T. ) ;
#4273 = EDGE_CURVE ( 'NONE', #3039, #3811, #12772, .T. ) ;
#4274 = CARTESIAN_POINT ( 'NONE',  ( 9.999999999999994671, 27.00000000000000000, -2.500000000000000000 ) ) ;
#4275 = VERTEX_POINT ( 'NONE', #5831 ) ;
#4276 = VECTOR ( 'NONE', #8277, 1000.000000000000000 ) ;
#4277 = CARTESIAN_POINT ( 'NONE',  ( 30.00000000000000711, 90.00000000000000000, -10.00000000000000000 ) ) ;
#4278 = VERTEX_POINT ( 'NONE', #3882 ) ;
#4279 = VECTOR ( 'NONE', #7353, 1000.000000000000000 ) ;
#4280 = CARTESIAN_POINT ( 'NONE',  ( 7.650000000000000355, 0.000000000000000000, 0.000000000000000000 ) ) ;
#4281 = CARTESIAN_POINT ( 'NONE',  ( 19.27821517812500574, 117.2309300971526937, 2.928125000614517415 ) ) ;
#4282 = CARTESIAN_POINT ( 'NONE',  ( 3.556430356250028790, 71.84604660189818048, 3.546875000614517326 ) ) ;
#4283 = CARTESIAN_POINT ( 'NONE',  ( 25.00000000000000355, -5.000000000000000000, 4.249999999999998224 ) ) ;
#4284 = CARTESIAN_POINT ( 'NONE',  ( 1.625004804578465745, -6.241943558307532669, -0.8000000000000000444 ) ) ;
#4285 = AXIS2_PLACEMENT_3D ( 'NONE', #5898, #4801, #12781 ) ;
#4286 = EDGE_CURVE ( 'NONE', #8362, #10857, #11427, .T. ) ;
#4287 = CIRCLE ( 'NONE', #10342, 1.599999999999998090 ) ;
#4288 = LINE ( 'NONE', #10164, #6146 ) ;
#4289 = EDGE_CURVE ( 'NONE', #10418, #11426, #1908, .T. ) ;
#4290 = DIRECTION ( 'NONE',  ( 1.000000000000000000, 0.000000000000000000, 0.000000000000000000 ) ) ;
#4291 = LINE ( 'NONE', #1204, #1121 ) ;
#4292 = LINE ( 'NONE', #5385, #939 ) ;
#4293 = DIRECTION ( 'NONE',  ( -1.000000000000000000, -0.000000000000000000, -0.000000000000000000 ) ) ;
#4294 = AXIS2_PLACEMENT_3D ( 'NONE', #4431, #6385, #11162 ) ;
#4295 = CARTESIAN_POINT ( 'NONE',  ( 19.27821517812500574, 117.2309300971526937, 3.434375000614517059 ) ) ;
#4296 = ORIENTED_EDGE ( 'NONE', *, *, #9492, .F. ) ;
#4297 = CIRCLE ( 'NONE', #8265, 1.000000000000000000 ) ;
#4298 = FACE_OUTER_BOUND ( 'NONE', #11649, .T. ) ;
#4299 = ORIENTED_EDGE ( 'NONE', *, *, #11783, .T. ) ;
#4300 = EDGE_CURVE ( 'NONE', #1050, #4594, #7914, .T. ) ;
#4301 = CARTESIAN_POINT ( 'NONE',  ( 8.500000000000000000, 71.85789451624832225, -1.000000000000000666 ) ) ;
#4302 = DIRECTION ( 'NONE',  ( 1.000000000000000000, 0.000000000000000000, 0.000000000000000000 ) ) ;
#4303 = DIRECTION ( 'NONE',  ( -0.000000000000000000, -0.000000000000000000, -1.000000000000000000 ) ) ;
#4304 = VECTOR ( 'NONE', #551, 1000.000000000000000 ) ;
#4305 = VERTEX_POINT ( 'NONE', #4666 ) ;
#4306 = DIRECTION ( 'NONE',  ( -0.000000000000000000, 1.000000000000000000, -0.000000000000000000 ) ) ;
#4307 = CARTESIAN_POINT ( 'NONE',  ( 22.99999999999998579, 90.00000000000000000, -8.000000000000000000 ) ) ;
#4308 = ORIENTED_EDGE ( 'NONE', *, *, #4684, .F. ) ;
#4309 = CARTESIAN_POINT ( 'NONE',  ( -63.73205080756886076, 30.46410161513775350, 0.000000000000000000 ) ) ;
#4310 = ORIENTED_EDGE ( 'NONE', *, *, #8400, .T. ) ;
#4312 = ORIENTED_EDGE ( 'NONE', *, *, #6671, .F. ) ;
#4311 = AXIS2_PLACEMENT_3D ( 'NONE', #2971, #12782, #993 ) ;
#4313 = AXIS2_PLACEMENT_3D ( 'NONE', #8168, #10188, #8365 ) ;
#4314 = CARTESIAN_POINT ( 'NONE',  ( 60.43447243729646345, 111.3420572890633764, 2.688859442485532991 ) ) ;
#4315 = LINE ( 'NONE', #9470, #11664 ) ;
#4316 = EDGE_LOOP ( 'NONE', ( #8648, #4133, #7628, #10875 ) ) ;
#4317 = EDGE_CURVE ( 'NONE', #5941, #10632, #8655, .T. ) ;
#4318 = VERTEX_POINT ( 'NONE', #10678 ) ;
#4319 = CARTESIAN_POINT ( 'NONE',  ( -48.33333333333332860, 0.000000000000000000, -1.734723475976807094E-15 ) ) ;
#4320 = ORIENTED_EDGE ( 'NONE', *, *, #8258, .T. ) ;
#4321 = CARTESIAN_POINT ( 'NONE',  ( 3.556430356250014579, 108.1539533981018053, 4.765625000614517326 ) ) ;
#4322 = ORIENTED_EDGE ( 'NONE', *, *, #12239, .F. ) ;
#4323 = CARTESIAN_POINT ( 'NONE',  ( 7.500000000000000000, 30.00000000000000000, 0.000000000000000000 ) ) ;
#4324 = EDGE_CURVE ( 'NONE', #8136, #5732, #1718, .T. ) ;
#4325 = VERTEX_POINT ( 'NONE', #7734 ) ;
#4326 = EDGE_CURVE ( 'NONE', #1479, #1569, #2771, .T. ) ;
#4327 = CARTESIAN_POINT ( 'NONE',  ( 1.040000000000000036, 0.5773502691896263972, 1.000000000000000000 ) ) ;
#4328 = PLANE ( 'NONE',  #10492 ) ;
#4329 = DIRECTION ( 'NONE',  ( 0.000000000000000000, 0.000000000000000000, -1.000000000000000000 ) ) ;
#4330 = SHAPE_REPRESENTATION_RELATIONSHIP ( 'NONE' , 'NONE' ,  #5582, #8095 ) ;
#4331 = VECTOR ( 'NONE', #7445, 1000.000000000000000 ) ;
#4332 = LINE ( 'NONE', #11567, #4356 ) ;
#4333 = VERTEX_POINT ( 'NONE', #5041 ) ;
#4334 = CARTESIAN_POINT ( 'NONE',  ( 3.800000000000015365, 90.00000000000000000, 4.549999999999999822 ) ) ;
#4335 = ORIENTED_EDGE ( 'NONE', *, *, #9302, .T. ) ;
#4336 = PLANE ( 'NONE',  #4180 ) ;
#4337 = EDGE_LOOP ( 'NONE', ( #10919, #2407 ) ) ;
#4338 = CARTESIAN_POINT ( 'NONE',  ( 9.650000000000000355, 1.493456771560197319E-16, -1.219500000000000028 ) ) ;
#4339 = ORIENTED_EDGE ( 'NONE', *, *, #1699, .T. ) ;
#4340 = CIRCLE ( 'NONE', #8308, 1.599999999999986766 ) ;
#4341 = DIRECTION ( 'NONE',  ( 1.000000000000000000, 0.000000000000000000, 0.000000000000000000 ) ) ;
#4342 = CARTESIAN_POINT ( 'NONE',  ( 9.999999999999994671, 27.00000000000000000, -2.500000000000000000 ) ) ;
#4343 = CARTESIAN_POINT ( 'NONE',  ( 66.44356964375000985, 71.84604660189820891, 3.246875000614517504 ) ) ;
#4344 = DIRECTION ( 'NONE',  ( 1.049727191973305517E-16, 0.5150380737757253025, -0.8571673013836857979 ) ) ;
#4345 = EDGE_CURVE ( 'NONE', #10785, #12605, #4821, .T. ) ;
#4346 = CARTESIAN_POINT ( 'NONE',  ( -60.00000000000000000, 30.00000000000000000, -3.000000000000000000 ) ) ;
#4347 = DIRECTION ( 'NONE',  ( -1.000000000000000000, 0.000000000000000000, 0.000000000000000000 ) ) ;
#4348 = VECTOR ( 'NONE', #10092, 1000.000000000000114 ) ;
#4349 = FACE_OUTER_BOUND ( 'NONE', #2942, .T. ) ;
#4350 = LINE ( 'NONE', #6914, #11472 ) ;
#4351 = DIRECTION ( 'NONE',  ( 0.000000000000000000, 0.000000000000000000, -1.000000000000000000 ) ) ;
#4352 = PLANE ( 'NONE',  #530 ) ;
#4353 = EDGE_CURVE ( 'NONE', #4553, #835, #5953, .T. ) ;
#4354 = CARTESIAN_POINT ( 'NONE',  ( 52.44898842787294768, 66.83414752756172561, 4.000000000000000000 ) ) ;
#4355 = CARTESIAN_POINT ( 'NONE',  ( 9.650000000000000355, 0.000000000000000000, 0.000000000000000000 ) ) ;
#4356 = VECTOR ( 'NONE', #5738, 1000.000000000000114 ) ;
#4357 = VERTEX_POINT ( 'NONE', #8964 ) ;
#4358 = AXIS2_PLACEMENT_3D ( 'NONE', #4055, #2027, #1960 ) ;
#4359 = PLANE ( 'NONE',  #9347 ) ;
#4360 = EDGE_LOOP ( 'NONE', ( #6330, #18, #11832, #4452 ) ) ;
#4361 = EDGE_CURVE ( 'NONE', #1810, #2828, #8027, .T. ) ;
#4362 = FILL_AREA_STYLE ('',( #1213 ) ) ;
#4363 = DIRECTION ( 'NONE',  ( 1.000000000000000000, 0.000000000000000000, 5.337610695313252124E-17 ) ) ;
#4364 = CARTESIAN_POINT ( 'NONE',  ( 45.00000000000000000, 2.000000000000000000, -4.150000000000005684 ) ) ;
#4365 = CARTESIAN_POINT ( 'NONE',  ( 17.55098605904792564, 66.83414348997642662, 1.000000000000003109 ) ) ;
#4366 = AXIS2_PLACEMENT_3D ( 'NONE', #10360, #10230, #9048 ) ;
#4367 = ORIENTED_EDGE ( 'NONE', *, *, #12144, .F. ) ;
#4368 = CARTESIAN_POINT ( 'NONE',  ( 1.040000000000000036, 0.5773502691896262862, -1.000000000000000000 ) ) ;
#4369 = CARTESIAN_POINT ( 'NONE',  ( 3.556430356250014579, 108.1539533981018053, 4.765625000614517326 ) ) ;
#4370 = ORIENTED_EDGE ( 'NONE', *, *, #7869, .F. ) ;
#4371 = LINE ( 'NONE', #10253, #12462 ) ;
#4372 = ORIENTED_EDGE ( 'NONE', *, *, #2781, .F. ) ;
#4373 = ADVANCED_FACE ( 'NONE', ( #8123 ), #10073, .F. ) ;
#4374 = VECTOR ( 'NONE', #9444, 1000.000000000000114 ) ;
#4375 = ORIENTED_EDGE ( 'NONE', *, *, #2075, .T. ) ;
#4376 = CIRCLE ( 'NONE', #5207, 29.99999999999999645 ) ;
#4377 = CARTESIAN_POINT ( 'NONE',  ( 7.500000000000000000, 30.00000000000000000, 0.000000000000000000 ) ) ;
#4378 = ORIENTED_EDGE ( 'NONE', *, *, #8402, .T. ) ;
#4379 = PRODUCT ( 'support', 'support', '', ( #6596 ) ) ;
#4380 = ORIENTED_EDGE ( 'NONE', *, *, #6829, .F. ) ;
#4382 = CARTESIAN_POINT ( 'NONE',  ( -28.99038105676692112, 50.21281292110204930, 1.000000000000000000 ) ) ;
#4381 = AXIS2_PLACEMENT_3D ( 'NONE', #5636, #4660, #3422 ) ;
#4383 = ORIENTED_EDGE ( 'NONE', *, *, #4161, .F. ) ;
#4384 = CARTESIAN_POINT ( 'NONE',  ( 56.62812188930148949, 112.6043444984596533, 3.000000000000000000 ) ) ;
#4385 = APPLICATION_PROTOCOL_DEFINITION ( 'draft international standard', 'automotive_design', 1998, #1590 ) ;
#4386 = CARTESIAN_POINT ( 'NONE',  ( 66.19999999999988916, 71.98667160128361786, 3.387499999999999734 ) ) ;
#4387 = ORIENTED_EDGE ( 'NONE', *, *, #4599, .F. ) ;
#4388 = CARTESIAN_POINT ( 'NONE',  ( 1.649999999999999911, 0.000000000000000000, 1.599999999999999645 ) ) ;
#4389 = ORIENTED_EDGE ( 'NONE', *, *, #9963, .T. ) ;
#4390 = ADVANCED_FACE ( 'NONE', ( #12678 ), #7671, .F. ) ;
#4391 = LINE ( 'NONE', #8186, #6923 ) ;
#4392 = CARTESIAN_POINT ( 'NONE',  ( 9.650000000000000355, 1.665213485140613626E-16, -1.219500000000000028 ) ) ;
#4393 = VECTOR ( 'NONE', #9992, 1000.000000000000000 ) ;
#4394 = FACE_BOUND ( 'NONE', #10586, .T. ) ;
#4395 = EDGE_CURVE ( 'NONE', #9287, #8977, #5660, .T. ) ;
#4397 = ADVANCED_FACE ( 'NONE', ( #11428, #10452 ), #4569, .F. ) ;
#4396 = VERTEX_POINT ( 'NONE', #5671 ) ;
#4398 = CARTESIAN_POINT ( 'NONE',  ( 50.72178482187501203, 62.76906990284730625, 4.109375000614517326 ) ) ;
#4399 = ORIENTED_EDGE ( 'NONE', *, *, #10311, .F. ) ;
#4400 = DIRECTION ( 'NONE',  ( -0.9510565162951529761, -0.3090169943749492276, 0.000000000000000000 ) ) ;
#4401 = VECTOR ( 'NONE', #8346, 1000.000000000000000 ) ;
#4402 = VECTOR ( 'NONE', #6368, 1000.000000000000000 ) ;
#4403 = CARTESIAN_POINT ( 'NONE',  ( 66.44356964374999563, 90.00000000000000000, 3.284375000614517148 ) ) ;
#4404 = EDGE_LOOP ( 'NONE', ( #590, #9688, #5701, #7390, #10772, #12756, #10894, #5883 ) ) ;
#4405 = DIRECTION ( 'NONE',  ( -0.000000000000000000, -0.000000000000000000, -1.000000000000000000 ) ) ;
#4406 = EDGE_CURVE ( 'NONE', #3143, #7972, #7701, .T. ) ;
#4407 = CARTESIAN_POINT ( 'NONE',  ( 4.030338320500828075, 95.53249351899766850, 2.999999999999999556 ) ) ;
#4408 = DIRECTION ( 'NONE',  ( -1.000000000000000000, -0.000000000000000000, -0.000000000000000000 ) ) ;
#4409 = CARTESIAN_POINT ( 'NONE',  ( 5.011331584521383498, 81.39071625125095011, 1.000000000000000000 ) ) ;
#4410 = CARTESIAN_POINT ( 'NONE',  ( 35.00000000000000000, 90.00000000000000000, -18.00000000000000355 ) ) ;
#4411 = VECTOR ( 'NONE', #541, 1000.000000000000000 ) ;
#4412 = DIRECTION ( 'NONE',  ( -0.000000000000000000, -0.000000000000000000, -1.000000000000000000 ) ) ;
#4413 = EDGE_CURVE ( 'NONE', #10818, #7686, #3718, .T. ) ;
#4414 = CARTESIAN_POINT ( 'NONE',  ( 35.00000000000000000, 90.00000000000000000, 4.000000000000000000 ) ) ;
#4415 = DIRECTION ( 'NONE',  ( 1.000000000000000000, 0.000000000000000000, 0.000000000000000000 ) ) ;
#4416 = CARTESIAN_POINT ( 'NONE',  ( -0.9999999999999997780, -4.273461295629625845, -0.8000000000000000444 ) ) ;
#4417 = DIRECTION ( 'NONE',  ( 0.000000000000000000, 0.000000000000000000, 1.000000000000000000 ) ) ;
#4418 = AXIS2_PLACEMENT_3D ( 'NONE', #3944, #7926, #11913 ) ;
#4419 = CARTESIAN_POINT ( 'NONE',  ( 45.00000000000000000, 2.000000000000001332, 4.150000000000010125 ) ) ;
#4420 = CARTESIAN_POINT ( 'NONE',  ( -60.00000000000000000, 0.000000000000000000, 9.999999999999996447 ) ) ;
#4421 = ORIENTED_EDGE ( 'NONE', *, *, #7379, .F. ) ;
#4422 = CARTESIAN_POINT ( 'NONE',  ( 34.25000000000000000, 92.49999999999998579, -8.000000000000000000 ) ) ;
#4423 = CARTESIAN_POINT ( 'NONE',  ( -23.49999999999999289, 53.38268590218009280, -1.000000000000000000 ) ) ;
#4424 = ORIENTED_EDGE ( 'NONE', *, *, #7958, .T. ) ;
#4425 = SURFACE_STYLE_USAGE ( .BOTH. , #8673 ) ;
#4426 = MECHANICAL_DESIGN_GEOMETRIC_PRESENTATION_REPRESENTATION (  '', ( #1070 ), #7764 ) ;
#4427 = FACE_OUTER_BOUND ( 'NONE', #2884, .T. ) ;
#4428 = CARTESIAN_POINT ( 'NONE',  ( 66.19999999999988916, 71.98667160128361786, 4.400000001229033231 ) ) ;
#4429 = DIRECTION ( 'NONE',  ( -0.000000000000000000, -0.000000000000000000, -1.000000000000000000 ) ) ;
#4430 = ORIENTED_EDGE ( 'NONE', *, *, #1875, .F. ) ;
#4431 = CARTESIAN_POINT ( 'NONE',  ( 35.00000000000000000, 90.00000000000000000, -8.000000000000000000 ) ) ;
#4432 = EDGE_CURVE ( 'NONE', #12789, #12512, #8497, .T. ) ;
#4433 = CARTESIAN_POINT ( 'NONE',  ( 1.649999999999999911, 0.000000000000000000, 0.000000000000000000 ) ) ;
#4434 = EDGE_LOOP ( 'NONE', ( #15, #12236, #7458, #4758 ) ) ;
#4435 = DIRECTION ( 'NONE',  ( 1.000000000000000000, 0.000000000000000000, 0.000000000000000000 ) ) ;
#4436 = DIRECTION ( 'NONE',  ( 1.000000000000000000, 0.000000000000000000, 0.000000000000000000 ) ) ;
#4437 = ORIENTED_EDGE ( 'NONE', *, *, #4217, .T. ) ;
#4438 = AXIS2_PLACEMENT_3D ( 'NONE', #4919, #8905, #10925 ) ;
#4439 = EDGE_LOOP ( 'NONE', ( #10915, #7711, #8975, #2361 ) ) ;
#4440 = DIRECTION ( 'NONE',  ( -0.000000000000000000, 1.000000000000000000, -0.000000000000000000 ) ) ;
#4441 = CARTESIAN_POINT ( 'NONE',  ( 35.00000000000000000, 90.00000000000000000, 4.000000000000000000 ) ) ;
#4442 = VERTEX_POINT ( 'NONE', #3527 ) ;
#4443 = EDGE_CURVE ( 'NONE', #10977, #12789, #12484, .T. ) ;
#4444 = ORIENTED_EDGE ( 'NONE', *, *, #1831, .T. ) ;
#4445 = CIRCLE ( 'NONE', #5279, 28.99999999999999289 ) ;
#4446 = LINE ( 'NONE', #2616, #7632 ) ;
#4447 = VERTEX_POINT ( 'NONE', #9662 ) ;
#4448 = FACE_OUTER_BOUND ( 'NONE', #12596, .T. ) ;
#4449 = ADVANCED_FACE ( 'NONE', ( #11493 ), #9724, .T. ) ;
#4450 = VERTEX_POINT ( 'NONE', #7509 ) ;
#4451 =( LENGTH_UNIT ( ) NAMED_UNIT ( * ) SI_UNIT ( .MILLI., .METRE. ) );
#4452 = ORIENTED_EDGE ( 'NONE', *, *, #11511, .T. ) ;
#4453 = SURFACE_SIDE_STYLE ('',( #577 ) ) ;
#4454 = EDGE_LOOP ( 'NONE', ( #2690, #6946, #6484, #10355 ) ) ;
#4455 = FACE_OUTER_BOUND ( 'NONE', #12847, .T. ) ;
#4456 = DIRECTION ( 'NONE',  ( -0.000000000000000000, 1.000000000000000000, -0.000000000000000000 ) ) ;
#4457 = AXIS2_PLACEMENT_3D ( 'NONE', #7107, #9066, #2278 ) ;
#4458 = EDGE_CURVE ( 'NONE', #4244, #370, #11851, .T. ) ;
#4459 = VERTEX_POINT ( 'NONE', #1685 ) ;
#4460 = CARTESIAN_POINT ( 'NONE',  ( 5.000000000000004441, 27.00000000000000000, -10.00000000000000000 ) ) ;
#4461 = ORIENTED_EDGE ( 'NONE', *, *, #4715, .F. ) ;
#4462 = DIRECTION ( 'NONE',  ( -0.5877852522924755796, -0.8090169943749457859, 0.000000000000000000 ) ) ;
#4463 = VERTEX_POINT ( 'NONE', #6648 ) ;
#4464 = CARTESIAN_POINT ( 'NONE',  ( 19.27821517812500574, 117.2309300971526937, 2.984375000614517326 ) ) ;
#4465 = ORIENTED_EDGE ( 'NONE', *, *, #5254, .T. ) ;
#4466 = DIRECTION ( 'NONE',  ( 1.000000000000000000, 0.000000000000000000, -0.000000000000000000 ) ) ;
#4467 = VECTOR ( 'NONE', #12474, 1000.000000000000000 ) ;
#4468 = CARTESIAN_POINT ( 'NONE',  ( 13.53859087060910404, 112.9805567844265539, 2.999999999999999112 ) ) ;
#4469 = CARTESIAN_POINT ( 'NONE',  ( 19.27821517812503060, 62.76906990284727783, 3.584375000614516971 ) ) ;
#4470 = CARTESIAN_POINT ( 'NONE',  ( 66.44356964374999563, 71.84604660189820891, 4.540625000614517681 ) ) ;
#4471 = LINE ( 'NONE', #10487, #4162 ) ;
#4472 = AXIS2_PLACEMENT_3D ( 'NONE', #296, #9792, #3915 ) ;
#4473 = PLANE ( 'NONE',  #9604 ) ;
#4474 = CARTESIAN_POINT ( 'NONE',  ( 35.00000000000000000, 90.00000000000000000, 22.38477631085024555 ) ) ;
#4475 = VECTOR ( 'NONE', #5260, 1000.000000000000000 ) ;
#4476 = PLANE ( 'NONE',  #7292 ) ;
#4477 = FACE_OUTER_BOUND ( 'NONE', #12786, .T. ) ;
#4478 = CIRCLE ( 'NONE', #8862, 3.351416843938787249 ) ;
#4479 = CARTESIAN_POINT ( 'NONE',  ( -43.33333333333332149, 39.62250448649387380, -1.000000000000000888 ) ) ;
#4480 = DIRECTION ( 'NONE',  ( 0.000000000000000000, 0.000000000000000000, 1.000000000000000000 ) ) ;
#4481 = LINE ( 'NONE', #7359, #2655 ) ;
#4483 = EDGE_CURVE ( 'NONE', #4357, #6677, #12483, .T. ) ;
#4482 = ORIENTED_EDGE ( 'NONE', *, *, #4582, .T. ) ;
#4484 = ADVANCED_FACE ( 'NONE', ( #562 ), #12553, .T. ) ;
#4485 = LINE ( 'NONE', #3203, #4647 ) ;
#4486 = PLANE ( 'NONE',  #5373 ) ;
#4487 = ORIENTED_EDGE ( 'NONE', *, *, #10221, .T. ) ;
#4488 = AXIS2_PLACEMENT_3D ( 'NONE', #4144, #1054, #5418 ) ;
#4489 = PRODUCT ( 'buckets', 'buckets', '', ( #8439 ) ) ;
#4490 = SURFACE_STYLE_FILL_AREA ( #9588 ) ;
#4491 = CIRCLE ( 'NONE', #3033, 4.000000000000000000 ) ;
#4492 = DIRECTION ( 'NONE',  ( -0.000000000000000000, -0.000000000000000000, -1.000000000000000000 ) ) ;
#4493 = LINE ( 'NONE', #1539, #316 ) ;
#4494 = CYLINDRICAL_SURFACE ( 'NONE', #9069, 31.19999999999998863 ) ;
#4495 = VERTEX_POINT ( 'NONE', #6712 ) ;
#4496 = AXIS2_PLACEMENT_3D ( 'NONE', #1220, #5212, #9202 ) ;
#4497 = DIRECTION ( 'NONE',  ( 0.000000000000000000, 0.8660254037844387076, 0.4999999999999998890 ) ) ;
#4498 = CARTESIAN_POINT ( 'NONE',  ( 50.72178482187501203, 62.76906990284730625, 4.503125000614517148 ) ) ;
#4499 = CIRCLE ( 'NONE', #2206, 31.20000000000000639 ) ;
#4500 = VERTEX_POINT ( 'NONE', #9466 ) ;
#4501 = DIRECTION ( 'NONE',  ( 0.000000000000000000, 0.000000000000000000, -1.000000000000000000 ) ) ;
#4502 = ORIENTED_EDGE ( 'NONE', *, *, #10990, .T. ) ;
#4503 = DIRECTION ( 'NONE',  ( -1.000000000000000000, 0.000000000000000000, 0.000000000000000000 ) ) ;
#4504 = ORIENTED_EDGE ( 'NONE', *, *, #10546, .F. ) ;
#4505 = DIRECTION ( 'NONE',  ( 0.000000000000000000, 0.000000000000000000, 1.000000000000000000 ) ) ;
#4506 = DIRECTION ( 'NONE',  ( 0.4719909656437444867, -0.8816033849473842166, 0.000000000000000000 ) ) ;
#4507 = CIRCLE ( 'NONE', #12855, 1.599999999999990319 ) ;
#4508 = EDGE_CURVE ( 'NONE', #6922, #6195, #3592, .T. ) ;
#4509 = ORIENTED_EDGE ( 'NONE', *, *, #976, .F. ) ;
#4510 = AXIS2_PLACEMENT_3D ( 'NONE', #8551, #12402, #5838 ) ;
#4511 = VERTEX_POINT ( 'NONE', #7573 ) ;
#4512 = CARTESIAN_POINT ( 'NONE',  ( -3.666666666666663410, 62.52406516434930239, -1.000000000000000888 ) ) ;
#4513 = ORIENTED_EDGE ( 'NONE', *, *, #7362, .T. ) ;
#4514 = CARTESIAN_POINT ( 'NONE',  ( 6.626776019045581556, 99.74475042915889844, -0.9999999999999970024 ) ) ;
#4515 = CARTESIAN_POINT ( 'NONE',  ( 48.49999999999995737, 94.00000000000000000, -10.00000000000000000 ) ) ;
#4516 = ORIENTED_EDGE ( 'NONE', *, *, #3056, .T. ) ;
#4517 =( REPRESENTATION_RELATIONSHIP ('NONE','NONE', #1997, #9523 ) REPRESENTATION_RELATIONSHIP_WITH_TRANSFORMATION ( #4895 )SHAPE_REPRESENTATION_RELATIONSHIP( ) );
#4518 = VECTOR ( 'NONE', #1529, 1000.000000000000000 ) ;
#4519 = ORIENTED_EDGE ( 'NONE', *, *, #5879, .F. ) ;
#4520 = VECTOR ( 'NONE', #10450, 1000.000000000000114 ) ;
#4521 = EDGE_CURVE ( 'NONE', #1894, #3861, #5733, .T. ) ;
#4522 = FILL_AREA_STYLE ('',( #3675 ) ) ;
#4523 = ORIENTED_EDGE ( 'NONE', *, *, #9782, .F. ) ;
#4524 = CARTESIAN_POINT ( 'NONE',  ( 31.55032196868182126, 58.90710318828558911, 3.000000000000000444 ) ) ;
#4525 = LINE ( 'NONE', #8448, #4564 ) ;
#4526 = EDGE_CURVE ( 'NONE', #11432, #1810, #628, .T. ) ;
#4527 = ORIENTED_EDGE ( 'NONE', *, *, #184, .T. ) ;
#4528 = VECTOR ( 'NONE', #11282, 1000.000000000000000 ) ;
#4529 = CARTESIAN_POINT ( 'NONE',  ( 66.44356964374998142, 108.1539533981018053, 3.771875000614516971 ) ) ;
#4530 = ORIENTED_EDGE ( 'NONE', *, *, #8611, .F. ) ;
#4531 = EDGE_LOOP ( 'NONE', ( #11178, #2768, #627, #12767, #2752 ) ) ;
#4532 = CARTESIAN_POINT ( 'NONE',  ( -6.666666666666660745, 0.000000000000000000, -1.499999999999999556 ) ) ;
#4533 = ORIENTED_EDGE ( 'NONE', *, *, #707, .T. ) ;
#4534 = FACE_OUTER_BOUND ( 'NONE', #9426, .T. ) ;
#4535 = LINE ( 'NONE', #9569, #2236 ) ;
#4536 = ADVANCED_FACE ( 'NONE', ( #1878 ), #9851, .T. ) ;
#4537 = AXIS2_PLACEMENT_3D ( 'NONE', #4101, #11083, #1207 ) ;
#4538 = CARTESIAN_POINT ( 'NONE',  ( 5.000000000000004441, 30.00000000000000000, -10.00000000000000000 ) ) ;
#4539 = CARTESIAN_POINT ( 'NONE',  ( 3.556430356250015024, 90.00000000000000000, 4.803125000614516971 ) ) ;
#4540 = CARTESIAN_POINT ( 'NONE',  ( 25.00000000000000355, 2.000000000000000000, 5.750000000000000000 ) ) ;
#4541 = CARTESIAN_POINT ( 'NONE',  ( 7.650000000000000355, 0.000000000000000000, 1.219500000000000028 ) ) ;
#4542 = LINE ( 'NONE', #10427, #5528 ) ;
#4543 = DIRECTION ( 'NONE',  ( 0.000000000000000000, 0.000000000000000000, -1.000000000000000000 ) ) ;
#4544 = DIRECTION ( 'NONE',  ( 0.000000000000000000, 0.000000000000000000, 1.000000000000000000 ) ) ;
#4545 = AXIS2_PLACEMENT_3D ( 'NONE', #5770, #8838, #9634 ) ;
#4546 = DIRECTION ( 'NONE',  ( -0.000000000000000000, -0.000000000000000000, -1.000000000000000000 ) ) ;
#4547 = CARTESIAN_POINT ( 'NONE',  ( 19.40000000000000924, 117.0199925980744666, 3.575000000000000178 ) ) ;
#4548 = DIRECTION ( 'NONE',  ( -1.000000000000000000, -0.000000000000000000, -0.000000000000000000 ) ) ;
#4549 = VERTEX_POINT ( 'NONE', #2988 ) ;
#4550 = EDGE_CURVE ( 'NONE', #4275, #1184, #8744, .T. ) ;
#4551 = DIRECTION ( 'NONE',  ( 0.000000000000000000, 0.000000000000000000, 1.000000000000000000 ) ) ;
#4552 = LINE ( 'NONE', #12598, #1834 ) ;
#4553 = VERTEX_POINT ( 'NONE', #880 ) ;
#4554 = CIRCLE ( 'NONE', #6626, 1.599999999999992095 ) ;
#4555 = CARTESIAN_POINT ( 'NONE',  ( 66.20000000000000284, 90.00000000000000000, 6.000000000000000000 ) ) ;
#4556 = CARTESIAN_POINT ( 'NONE',  ( 1.040000000000000036, 1.154700538379252350, -1.084202172485497162E-16 ) ) ;
#4557 = EDGE_CURVE ( 'NONE', #8368, #4056, #7777, .T. ) ;
#4558 = CARTESIAN_POINT ( 'NONE',  ( 66.19999999999988916, 71.98667160128361786, 3.050000001229034030 ) ) ;
#4559 = ADVANCED_FACE ( 'NONE', ( #4883 ), #8872, .F. ) ;
#4560 = ORIENTED_EDGE ( 'NONE', *, *, #531, .T. ) ;
#4561 = DIRECTION ( 'NONE',  ( -0.000000000000000000, -0.000000000000000000, -1.000000000000000000 ) ) ;
#4562 = AXIS2_PLACEMENT_3D ( 'NONE', #3598, #4703, #7643 ) ;
#4563 = DIRECTION ( 'NONE',  ( 0.000000000000000000, 0.000000000000000000, 1.000000000000000000 ) ) ;
#4564 = VECTOR ( 'NONE', #11516, 1000.000000000000000 ) ;
#4565 = ORIENTED_EDGE ( 'NONE', *, *, #7521, .F. ) ;
#4566 = DIRECTION ( 'NONE',  ( 0.000000000000000000, 0.000000000000000000, 1.000000000000000000 ) ) ;
#4567 = FACE_OUTER_BOUND ( 'NONE', #3287, .T. ) ;
#4568 = ORIENTED_EDGE ( 'NONE', *, *, #791, .T. ) ;
#4569 = PLANE ( 'NONE',  #1610 ) ;
#4570 = ORIENTED_EDGE ( 'NONE', *, *, #10835, .F. ) ;
#4571 = CARTESIAN_POINT ( 'NONE',  ( 30.00000000000000711, 90.00000000000000000, -5.000000000000000000 ) ) ;
#4572 = CARTESIAN_POINT ( 'NONE',  ( 45.00000000000000000, -5.000000000000000000, 7.250000000000001776 ) ) ;
#4573 = ORIENTED_EDGE ( 'NONE', *, *, #4652, .T. ) ;
#4574 = AXIS2_PLACEMENT_3D ( 'NONE', #5222, #10001, #10060 ) ;
#4575 = CARTESIAN_POINT ( 'NONE',  ( -6.666666666666660745, 0.000000000000000000, -1.499999999999999556 ) ) ;
#4576 = ORIENTED_EDGE ( 'NONE', *, *, #11395, .T. ) ;
#4577 = DIRECTION ( 'NONE',  ( -5.624500927088228034E-17, 1.370729058197317775E-18, 1.000000000000000000 ) ) ;
#4578 = VERTEX_POINT ( 'NONE', #17 ) ;
#4579 = DIRECTION ( 'NONE',  ( 0.000000000000000000, 0.000000000000000000, 1.000000000000000000 ) ) ;
#4580 = CARTESIAN_POINT ( 'NONE',  ( 3.800000000000015810, 108.0133283987162969, 4.625000001229034652 ) ) ;
#4581 = ORIENTED_EDGE ( 'NONE', *, *, #6194, .T. ) ;
#4582 = EDGE_CURVE ( 'NONE', #3017, #36, #2798, .T. ) ;
#4583 = CARTESIAN_POINT ( 'NONE',  ( 1.617350269189632428, 0.000000000000000000, 0.000000000000000000 ) ) ;
#4584 = VERTEX_POINT ( 'NONE', #12866 ) ;
#4585 = VECTOR ( 'NONE', #11137, 1000.000000000000000 ) ;
#4586 = ORIENTED_EDGE ( 'NONE', *, *, #7865, .F. ) ;
#4587 = CARTESIAN_POINT ( 'NONE',  ( 14.31119263734989033, 66.46175970803329847, 3.000000000000000444 ) ) ;
#4588 = FACE_BOUND ( 'NONE', #11738, .T. ) ;
#4589 = CIRCLE ( 'NONE', #2085, 1.499999999999999556 ) ;
#4590 = VECTOR ( 'NONE', #6285, 1000.000000000000000 ) ;
#4591 = VERTEX_POINT ( 'NONE', #945 ) ;
#4592 = CARTESIAN_POINT ( 'NONE',  ( 35.00000000000000711, 53.69209320379640360, 3.171875000614517326 ) ) ;
#4593 = EDGE_CURVE ( 'NONE', #10173, #11250, #8933, .T. ) ;
#4594 = VERTEX_POINT ( 'NONE', #6969 ) ;
#4595 = FACE_OUTER_BOUND ( 'NONE', #12141, .T. ) ;
#4596 = EDGE_LOOP ( 'NONE', ( #5931, #9274 ) ) ;
#4597 = SHAPE_REPRESENTATION ( 'socket button head screw_iso_ISO 7380 - M3 x 8 - 8N', ( #5704 ), #11138 ) ;
#4598 = CARTESIAN_POINT ( 'NONE',  ( 35.00000000000000000, 126.3079067962035822, 3.396875000614517415 ) ) ;
#4599 = EDGE_CURVE ( 'NONE', #5406, #12152, #12929, .T. ) ;
#4600 = ORIENTED_EDGE ( 'NONE', *, *, #3904, .T. ) ;
#4601 = AXIS2_PLACEMENT_3D ( 'NONE', #7047, #9004, #5213 ) ;
#4602 = CARTESIAN_POINT ( 'NONE',  ( 40.00000000000000000, 121.2009999999999934, 1.500000000000001110 ) ) ;
#4603 = CARTESIAN_POINT ( 'NONE',  ( 12.08740047754302616, 111.5578937668422270, 3.000000000000000888 ) ) ;
#4604 =( NAMED_UNIT ( * ) PLANE_ANGLE_UNIT ( ) SI_UNIT ( $, .RADIAN. ) );
#4605 = CARTESIAN_POINT ( 'NONE',  ( 3.800000000000015365, 90.00000000000000000, 3.312500001229034652 ) ) ;
#4606 = FACE_OUTER_BOUND ( 'NONE', #3725, .T. ) ;
#4607 = DIRECTION ( 'NONE',  ( -1.000000000000000000, 0.000000000000000000, 0.000000000000000000 ) ) ;
#4608 = VECTOR ( 'NONE', #1274, 1000.000000000000227 ) ;
#4609 = CARTESIAN_POINT ( 'NONE',  ( 1.000000000000000000, -4.873461295629625489, -0.8000000000000000444 ) ) ;
#4610 = ADVANCED_FACE ( 'NONE', ( #11752, #9790, #6779, #10771 ), #6906, .F. ) ;
#4611 = CARTESIAN_POINT ( 'NONE',  ( 18.35873618070580093, 66.24461453698026503, -1.000000000000000000 ) ) ;
#4612 = DIRECTION ( 'NONE',  ( 0.4999999999999985012, -0.8660254037844394848, -0.000000000000000000 ) ) ;
#4613 = LINE ( 'NONE', #1728, #4518 ) ;
#4614 = EDGE_CURVE ( 'NONE', #10459, #12299, #6199, .T. ) ;
#4615 = CARTESIAN_POINT ( 'NONE',  ( -3.350000000000000089, 4.102566777143633281E-16, -0.8000000000000000444 ) ) ;
#4616 = DIRECTION ( 'NONE',  ( 1.301042606982605124E-15, 7.511572993685881931E-16, 1.000000000000000000 ) ) ;
#4617 = ORIENTED_EDGE ( 'NONE', *, *, #10184, .F. ) ;
#4618 = CARTESIAN_POINT ( 'NONE',  ( 35.00000000000000711, 53.97334320256736362, 3.762500000000000178 ) ) ;
#4619 = VECTOR ( 'NONE', #8790, 1000.000000000000114 ) ;
#4620 = DIRECTION ( 'NONE',  ( 0.000000000000000000, -0.000000000000000000, 1.000000000000000000 ) ) ;
#4621 = ORIENTED_EDGE ( 'NONE', *, *, #1518, .F. ) ;
#4622 = DIRECTION ( 'NONE',  ( -0.000000000000000000, -0.000000000000000000, -1.000000000000000000 ) ) ;
#4623 = ADVANCED_FACE ( 'NONE', ( #5984 ), #4822, .F. ) ;
#4624 = CARTESIAN_POINT ( 'NONE',  ( 35.75000000000000711, 93.50000000000000000, 4.000000000000000000 ) ) ;
#4625 = VECTOR ( 'NONE', #9173, 1000.000000000000000 ) ;
#4626 = ORIENTED_EDGE ( 'NONE', *, *, #10354, .T. ) ;
#4627 = DIRECTION ( 'NONE',  ( 0.8660254037844361541, 0.5000000000000042188, -9.389466242107221759E-17 ) ) ;
#4628 = CARTESIAN_POINT ( 'NONE',  ( 3.556430356250015024, 90.00000000000000000, 4.353125000614517681 ) ) ;
#4629 = ORIENTED_EDGE ( 'NONE', *, *, #3390, .F. ) ;
#4630 = DIRECTION ( 'NONE',  ( 1.000000000000000000, 0.000000000000000000, -0.000000000000000000 ) ) ;
#4631 = DIRECTION ( 'NONE',  ( -0.000000000000000000, -0.000000000000000000, -1.000000000000000000 ) ) ;
#4632 = EDGE_LOOP ( 'NONE', ( #305, #8686, #7211, #4629 ) ) ;
#4633 = DIRECTION ( 'NONE',  ( 0.000000000000000000, 0.000000000000000000, 1.000000000000000000 ) ) ;
#4634 = VERTEX_POINT ( 'NONE', #1010 ) ;
#4635 = EDGE_CURVE ( 'NONE', #3826, #12707, #2071, .T. ) ;
#4636 = CARTESIAN_POINT ( 'NONE',  ( 3.000000000000004441, 30.00000000000000000, 0.000000000000000000 ) ) ;
#4637 = VECTOR ( 'NONE', #658, 1000.000000000000000 ) ;
#4638 = CARTESIAN_POINT ( 'NONE',  ( 46.89999999999997016, 90.00000000000000000, -8.000000000000000000 ) ) ;
#4639 = CARTESIAN_POINT ( 'NONE',  ( -60.00000000000000000, 30.00000000000000000, -0.9999999999999947820 ) ) ;
#4640 = CARTESIAN_POINT ( 'NONE',  ( 21.49999999999998579, 86.00000000000000000, -8.000000000000000000 ) ) ;
#4641 = DIRECTION ( 'NONE',  ( -1.000000000000000000, 0.000000000000000000, 0.000000000000000000 ) ) ;
#4642 = EDGE_LOOP ( 'NONE', ( #8885, #2588, #12089 ) ) ;
#4643 = CARTESIAN_POINT ( 'NONE',  ( -0.2000000000000000111, -6.446898479113814417, 0.000000000000000000 ) ) ;
#4644 = CONTEXT_DEPENDENT_SHAPE_REPRESENTATION ( #3431, #723 ) ;
#4645 = CARTESIAN_POINT ( 'NONE',  ( 66.19999999999997442, 108.0133283987163253, 3.125000001229034208 ) ) ;
#4646 = ORIENTED_EDGE ( 'NONE', *, *, #9208, .T. ) ;
#4647 = VECTOR ( 'NONE', #9387, 1000.000000000000000 ) ;
#4648 = SURFACE_STYLE_FILL_AREA ( #12629 ) ;
#4649 = ORIENTED_EDGE ( 'NONE', *, *, #8701, .T. ) ;
#4650 = EDGE_LOOP ( 'NONE', ( #6615, #2415, #9300, #4322 ) ) ;
#4651 = EDGE_CURVE ( 'NONE', #8770, #4892, #9964, .T. ) ;
#4652 = EDGE_CURVE ( 'NONE', #5149, #6677, #12800, .T. ) ;
#4653 = PLANE ( 'NONE',  #11336 ) ;
#4654 = DIRECTION ( 'NONE',  ( -0.000000000000000000, -0.000000000000000000, 1.000000000000000000 ) ) ;
#4655 = UNCERTAINTY_MEASURE_WITH_UNIT (LENGTH_MEASURE( 1.000000000000000082E-05 ), #3024, 'distance_accuracy_value', 'NONE');
#4656 = COLOUR_RGB ( '',1.000000000000000000, 0.9490196078431372140, 0.9098039215686274384 ) ;
#4657 = ORIENTED_EDGE ( 'NONE', *, *, #3785, .T. ) ;
#4658 = CARTESIAN_POINT ( 'NONE',  ( 19.27821517812503060, 62.76906990284727783, 3.584375000614516971 ) ) ;
#4659 = VERTEX_POINT ( 'NONE', #11820 ) ;
#4660 = DIRECTION ( 'NONE',  ( 5.337610695313252124E-17, 0.000000000000000000, -1.000000000000000000 ) ) ;
#4661 = ORIENTED_EDGE ( 'NONE', *, *, #4687, .T. ) ;
#4662 = CARTESIAN_POINT ( 'NONE',  ( 19.27821517812503060, 62.76906990284727783, 4.484375000614516438 ) ) ;
#4663 = ORIENTED_EDGE ( 'NONE', *, *, #2733, .T. ) ;
#4664 = VECTOR ( 'NONE', #2010, 1000.000000000000000 ) ;
#4665 = CARTESIAN_POINT ( 'NONE',  ( 46.98957880828161393, 117.5000000000000711, 1.000000000000003553 ) ) ;
#4666 = CARTESIAN_POINT ( 'NONE',  ( -43.33333333333332860, 41.93190556325237850, 1.000000000000000000 ) ) ;
#4667 = CARTESIAN_POINT ( 'NONE',  ( 1.749999999999999112, 1.959434878635763504E-16, -1.599999999999998757 ) ) ;
#4668 = DIRECTION ( 'NONE',  ( -1.000000000000000000, 0.000000000000000000, 0.000000000000000000 ) ) ;
#4669 = PLANE ( 'NONE',  #2302 ) ;
#4670 = ADVANCED_FACE ( 'NONE', ( #6841 ), #12075, .T. ) ;
#4671 = PRESENTATION_LAYER_ASSIGNMENT (  '', '', ( #1945 ) ) ;
#4672 = CARTESIAN_POINT ( 'NONE',  ( -16.33333333333332504, 2.000000000000000000, 7.999999999999996447 ) ) ;
#4673 = DIRECTION ( 'NONE',  ( -0.000000000000000000, -0.000000000000000000, -1.000000000000000000 ) ) ;
#4674 = DIRECTION ( 'NONE',  ( 0.000000000000000000, 0.000000000000000000, -1.000000000000000000 ) ) ;
#4675 = VECTOR ( 'NONE', #10712, 1000.000000000000227 ) ;
#4676 = CARTESIAN_POINT ( 'NONE',  ( 25.00000000000000355, -5.000000000000000000, 5.750000000000000000 ) ) ;
#4677 = CARTESIAN_POINT ( 'NONE',  ( 1.750000000000000000, 1.836970198721029441E-16, -1.499999999999999556 ) ) ;
#4678 = FACE_OUTER_BOUND ( 'NONE', #2890, .T. ) ;
#4679 = EDGE_LOOP ( 'NONE', ( #1244, #11959, #7907, #3611 ) ) ;
#4680 = CARTESIAN_POINT ( 'NONE',  ( 66.19999999999997442, 108.0133283987163253, 3.462499999999999911 ) ) ;
#4681 = ADVANCED_FACE ( 'NONE', ( #4298 ), #5267, .F. ) ;
#4682 = DIRECTION ( 'NONE',  ( -0.000000000000000000, 1.000000000000000000, -0.000000000000000000 ) ) ;
#4683 = ORIENTED_EDGE ( 'NONE', *, *, #11546, .F. ) ;
#4684 = EDGE_CURVE ( 'NONE', #1986, #7217, #5136, .T. ) ;
#4685 = DIRECTION ( 'NONE',  ( 0.000000000000000000, 0.000000000000000000, 1.000000000000000000 ) ) ;
#4686 = VECTOR ( 'NONE', #2745, 1000.000000000000000 ) ;
#4687 = EDGE_CURVE ( 'NONE', #5750, #4968, #3121, .T. ) ;
#4688 = DIRECTION ( 'NONE',  ( 0.000000000000000000, 0.000000000000000000, 1.000000000000000000 ) ) ;
#4689 = LINE ( 'NONE', #10577, #1755 ) ;
#4690 = AXIS2_PLACEMENT_3D ( 'NONE', #5205, #5269, #1340 ) ;
#4691 = ORIENTED_EDGE ( 'NONE', *, *, #8088, .F. ) ;
#4692 = DIRECTION ( 'NONE',  ( -1.000000000000000000, 0.000000000000000000, 0.000000000000000000 ) ) ;
#4693 = CARTESIAN_POINT ( 'NONE',  ( 66.44356964374999563, 90.00000000000000000, 3.678125000614516971 ) ) ;
#4694 = DIRECTION ( 'NONE',  ( -0.000000000000000000, -0.000000000000000000, -1.000000000000000000 ) ) ;
#4695 = AXIS2_PLACEMENT_3D ( 'NONE', #10167, #2064, #341 ) ;
#4696 = LINE ( 'NONE', #5608, #4520 ) ;
#4697 = VERTEX_POINT ( 'NONE', #1211 ) ;
#4698 = DIRECTION ( 'NONE',  ( 0.000000000000000000, 0.000000000000000000, -1.000000000000000000 ) ) ;
#4699 = ORIENTED_EDGE ( 'NONE', *, *, #8839, .F. ) ;
#4700 = EDGE_CURVE ( 'NONE', #36, #5747, #1400, .T. ) ;
#4701 = CARTESIAN_POINT ( 'NONE',  ( 2.387319993259524598, -4.036502139894371233, -0.8000000000000000444 ) ) ;
#4702 = CARTESIAN_POINT ( 'NONE',  ( 5.000000000000004441, 76.58915998087155685, 2.500000000000000444 ) ) ;
#4703 = DIRECTION ( 'NONE',  ( 0.000000000000000000, 0.000000000000000000, -1.000000000000000000 ) ) ;
#4704 = DIRECTION ( 'NONE',  ( 0.000000000000000000, 0.000000000000000000, 1.000000000000000000 ) ) ;
#4705 = AXIS2_PLACEMENT_3D ( 'NONE', #9049, #11211, #1267 ) ;
#4706 = FACE_OUTER_BOUND ( 'NONE', #8283, .T. ) ;
#4707 = ORIENTED_EDGE ( 'NONE', *, *, #11101, .T. ) ;
#4708 = DIRECTION ( 'NONE',  ( -0.000000000000000000, 1.000000000000000000, -0.000000000000000000 ) ) ;
#4709 = CONTEXT_DEPENDENT_SHAPE_REPRESENTATION ( #7181, #11694 ) ;
#4710 = DIRECTION ( 'NONE',  ( 1.000000000000000000, 0.000000000000000000, 5.337610695313252124E-17 ) ) ;
#4711 = ORIENTED_EDGE ( 'NONE', *, *, #3331, .F. ) ;
#4712 = ORIENTED_EDGE ( 'NONE', *, *, #11454, .T. ) ;
#4714 = ORIENTED_EDGE ( 'NONE', *, *, #6460, .F. ) ;
#4713 = VECTOR ( 'NONE', #2343, 1000.000000000000000 ) ;
#4715 = EDGE_CURVE ( 'NONE', #7663, #1018, #5331, .T. ) ;
#4716 = AXIS2_PLACEMENT_3D ( 'NONE', #5353, #9348, #8504 ) ;
#4717 = CARTESIAN_POINT ( 'NONE',  ( 9.181393010286774015, 72.18334839091693311, 3.000000000000002220 ) ) ;
#4718 = CARTESIAN_POINT ( 'NONE',  ( 35.00000000000000711, 53.97334320256736362, 3.312500000000000000 ) ) ;
#4719 = ORIENTED_EDGE ( 'NONE', *, *, #10822, .F. ) ;
#4720 = CARTESIAN_POINT ( 'NONE',  ( -31.49999999999998579, 79.07477288111861924, -1.000000000000000000 ) ) ;
#4721 = EDGE_LOOP ( 'NONE', ( #1992, #8667, #7049, #12501, #6935 ) ) ;
#4722 = VECTOR ( 'NONE', #3250, 999.9999999999998863 ) ;
#4723 = EDGE_CURVE ( 'NONE', #1427, #992, #9128, .T. ) ;
#4724 = DIRECTION ( 'NONE',  ( 0.000000000000000000, -1.000000000000000000, 0.000000000000000000 ) ) ;
#4725 = EDGE_CURVE ( 'NONE', #7369, #4634, #6112, .T. ) ;
#4726 = ORIENTED_EDGE ( 'NONE', *, *, #7635, .T. ) ;
#4727 = CARTESIAN_POINT ( 'NONE',  ( 3.556430356250028790, 71.84604660189818048, 3.040625000614517237 ) ) ;
#4728 = VERTEX_POINT ( 'NONE', #10106 ) ;
#4729 = DIRECTION ( 'NONE',  ( 0.000000000000000000, 0.000000000000000000, 1.000000000000000000 ) ) ;
#4730 = CARTESIAN_POINT ( 'NONE',  ( 50.59999999999999432, 117.0199925980744666, 3.950000000000000178 ) ) ;
#4731 = SURFACE_SIDE_STYLE ('',( #11789 ) ) ;
#4732 = CARTESIAN_POINT ( 'NONE',  ( 50.60000000000001563, 62.98000740192552627, 4.362500001229034474 ) ) ;
#4733 = COLOUR_RGB ( '',1.000000000000000000, 0.9490196078431372140, 0.9098039215686274384 ) ;
#4734 = PLANE ( 'NONE',  #7090 ) ;
#4735 = LINE ( 'NONE', #1982, #2615 ) ;
#4736 = CARTESIAN_POINT ( 'NONE',  ( 7.576448291486922670, 99.43666122937791840, 4.000000000000000000 ) ) ;
#4737 = CARTESIAN_POINT ( 'NONE',  ( 18.35999869903453430, 66.24638416994363865, 4.000000000000000000 ) ) ;
#4738 = CARTESIAN_POINT ( 'NONE',  ( 64.54729015011659499, 100.7543347877113717, 2.840101390178781049 ) ) ;
#4739 = AXIS2_PLACEMENT_3D ( 'NONE', #4033, #5795, #11938 ) ;
#4740 = DIRECTION ( 'NONE',  ( 0.000000000000000000, -1.000000000000000000, 0.000000000000000000 ) ) ;
#4741 = CARTESIAN_POINT ( 'NONE',  ( 3.556430356250015024, 90.00000000000000000, 3.059375000614517059 ) ) ;
#4742 = EDGE_CURVE ( 'NONE', #718, #6649, #11085, .T. ) ;
#4743 = VERTEX_POINT ( 'NONE', #12337 ) ;
#4744 = CARTESIAN_POINT ( 'NONE',  ( 3.800000000000025135, 71.98667160128366049, 4.137500000000001066 ) ) ;
#4745 = DIRECTION ( 'NONE',  ( 1.000000000000000000, 0.000000000000000000, 5.337610695313252124E-17 ) ) ;
#4746 = EDGE_LOOP ( 'NONE', ( #6394, #7273, #2614, #5268 ) ) ;
#4747 = DIRECTION ( 'NONE',  ( 0.000000000000000000, 0.000000000000000000, 1.000000000000000000 ) ) ;
#4748 =( BOUNDED_CURVE ( )  B_SPLINE_CURVE ( 2, ( #11721, #7670, #12899, #11850, #4730, #8715, #6875 ),
 .UNSPECIFIED., .F., .F. ) 
 B_SPLINE_CURVE_WITH_KNOTS ( ( 3, 2, 2, 3 ),
 ( 0.3999999999999999667, 0.4333333333333333481, 0.4666666666666667296, 0.5000000000000001110 ),
 .UNSPECIFIED. ) 
 CURVE ( )  GEOMETRIC_REPRESENTATION_ITEM ( )  RATIONAL_B_SPLINE_CURVE ( ( 1.000000000000000444, 0.8660254037844385966, 1.000000000000000000, 0.8660254037844387076, 1.000000000000000000, 0.8660254037844382635, 1.000000000000000444 ) ) 
 REPRESENTATION_ITEM ( '' )  );
#4749 = VECTOR ( 'NONE', #7102, 1000.000000000000114 ) ;
#4750 = DIRECTION ( 'NONE',  ( -0.000000000000000000, -0.5000000000000003331, 0.8660254037844384856 ) ) ;
#4751 = CARTESIAN_POINT ( 'NONE',  ( 1.040000000000000036, 0.000000000000000000, 0.000000000000000000 ) ) ;
#4752 = EDGE_CURVE ( 'NONE', #6664, #5149, #4554, .T. ) ;
#4753 = CARTESIAN_POINT ( 'NONE',  ( 25.83484861008832567, 86.00000000000000000, -8.000000000000000000 ) ) ;
#4754 = DIRECTION ( 'NONE',  ( 0.000000000000000000, 0.000000000000000000, 1.000000000000000000 ) ) ;
#4755 = CARTESIAN_POINT ( 'NONE',  ( 0.000000000000000000, 0.5773502691896263972, -1.000000000000000000 ) ) ;
#4756 = CARTESIAN_POINT ( 'NONE',  ( 35.00000000000000711, 53.69209320379639649, 4.521875000614516971 ) ) ;
#4757 = ADVANCED_FACE ( 'NONE', ( #9059 ), #3384, .F. ) ;
#4758 = ORIENTED_EDGE ( 'NONE', *, *, #6379, .F. ) ;
#4759 = VECTOR ( 'NONE', #4745, 1000.000000000000000 ) ;
#4760 = CARTESIAN_POINT ( 'NONE',  ( 8.923698042205888470, 69.79311561821251075, -2.500000000000000000 ) ) ;
#4761 = ORIENTED_EDGE ( 'NONE', *, *, #3963, .F. ) ;
#4762 = CARTESIAN_POINT ( 'NONE',  ( 0.000000000000000000, 0.000000000000000000, 0.000000000000000000 ) ) ;
#4763 =( REPRESENTATION_RELATIONSHIP ('NONE','NONE', #1997, #9937 ) REPRESENTATION_RELATIONSHIP_WITH_TRANSFORMATION ( #10399 )SHAPE_REPRESENTATION_RELATIONSHIP( ) );
#4764 = PLANE ( 'NONE',  #12503 ) ;
#4765 = DIRECTION ( 'NONE',  ( -1.000000000000000000, 0.000000000000000000, 0.000000000000000000 ) ) ;
#4766 = ORIENTED_EDGE ( 'NONE', *, *, #7692, .T. ) ;
#4767 = AXIS2_PLACEMENT_3D ( 'NONE', #9572, #2451, #6555 ) ;
#4768 = DIRECTION ( 'NONE',  ( 0.000000000000000000, 0.000000000000000000, -1.000000000000000000 ) ) ;
#4769 = ORIENTED_EDGE ( 'NONE', *, *, #6371, .F. ) ;
#4770 = LINE ( 'NONE', #6658, #12645 ) ;
#4771 = DIRECTION ( 'NONE',  ( -0.000000000000000000, 1.000000000000000000, -0.000000000000000000 ) ) ;
#4772 = ADVANCED_FACE ( 'NONE', ( #2136, #215 ), #4359, .F. ) ;
#4773 = ORIENTED_EDGE ( 'NONE', *, *, #184, .F. ) ;
#4774 = SURFACE_SIDE_STYLE ('',( #7908 ) ) ;
#4775 = ORIENTED_EDGE ( 'NONE', *, *, #8076, .F. ) ;
#4776 = ORIENTED_EDGE ( 'NONE', *, *, #9631, .F. ) ;
#4777 = VECTOR ( 'NONE', #9984, 1000.000000000000000 ) ;
#4778 = AXIS2_PLACEMENT_3D ( 'NONE', #5476, #1492, #7254 ) ;
#4779 = CARTESIAN_POINT ( 'NONE',  ( 3.557912590344627368, 88.92516271332206657, 3.000000000000001776 ) ) ;
#4780 = LINE ( 'NONE', #5820, #6861 ) ;
#4781 = VERTEX_POINT ( 'NONE', #2337 ) ;
#4782 = CARTESIAN_POINT ( 'NONE',  ( 1.040000000000000036, -1.154700538379251684, -1.199226976249124676E-17 ) ) ;
#4783 = VERTEX_POINT ( 'NONE', #7299 ) ;
#4784 = CARTESIAN_POINT ( 'NONE',  ( 3.556430356250015024, 90.00000000000000000, 4.803125000614516971 ) ) ;
#4785 = ADVANCED_FACE ( 'NONE', ( #150 ), #87, .F. ) ;
#4786 = ORIENTED_EDGE ( 'NONE', *, *, #2930, .F. ) ;
#4787 = CARTESIAN_POINT ( 'NONE',  ( 50.72178482187499071, 117.2309300971526937, 4.203125000614517326 ) ) ;
#4788 = VERTEX_POINT ( 'NONE', #4167 ) ;
#4789 = DIRECTION ( 'NONE',  ( 0.000000000000000000, 0.000000000000000000, 1.000000000000000000 ) ) ;
#4790 = DIRECTION ( 'NONE',  ( 0.5877852522924715828, 0.8090169943749485615, 0.000000000000000000 ) ) ;
#4791 = CYLINDRICAL_SURFACE ( 'NONE', #3191, 3.349999999999995204 ) ;
#4792 = VECTOR ( 'NONE', #12749, 1000.000000000000000 ) ;
#4793 = CARTESIAN_POINT ( 'NONE',  ( 19.27821517812500574, 117.2309300971526937, 3.378125000614517148 ) ) ;
#4794 = EDGE_CURVE ( 'NONE', #8071, #3015, #7363, .T. ) ;
#4795 = AXIS2_PLACEMENT_3D ( 'NONE', #12247, #11120, #3294 ) ;
#4796 = ADVANCED_FACE ( 'NONE', ( #11346 ), #12142, .T. ) ;
#4797 = CARTESIAN_POINT ( 'NONE',  ( 5.000000000000004441, 30.00000000000000000, -10.00000000000000000 ) ) ;
#4798 = DIRECTION ( 'NONE',  ( -0.000000000000000000, -0.000000000000000000, -1.000000000000000000 ) ) ;
#4799 = CARTESIAN_POINT ( 'NONE',  ( 66.19999999999998863, 90.00000000000000000, 5.000000000000000000 ) ) ;
#4800 = DIRECTION ( 'NONE',  ( 0.5000000000000036637, -0.8660254037844365982, 0.000000000000000000 ) ) ;
#4801 = DIRECTION ( 'NONE',  ( 0.000000000000000000, 0.000000000000000000, -1.000000000000000000 ) ) ;
#4802 = AXIS2_PLACEMENT_3D ( 'NONE', #8774, #1968, #7919 ) ;
#4803 = EDGE_CURVE ( 'NONE', #3214, #703, #10243, .T. ) ;
#4804 = CYLINDRICAL_SURFACE ( 'NONE', #1591, 6.499999999999999112 ) ;
#4805 = CARTESIAN_POINT ( 'NONE',  ( 1.040000000000000036, 0.5773502691896262862, 1.000000000000000000 ) ) ;
#4806 = CARTESIAN_POINT ( 'NONE',  ( 64.54728994471078352, 100.7543353520590870, 2.858851390178780871 ) ) ;
#4807 = VERTEX_POINT ( 'NONE', #4423 ) ;
#4808 = CARTESIAN_POINT ( 'NONE',  ( 35.00000000000000000, 126.0266567974326222, 3.987499999999999378 ) ) ;
#4809 = LINE ( 'NONE', #5908, #6840 ) ;
#4810 = ORIENTED_EDGE ( 'NONE', *, *, #3697, .T. ) ;
#4811 = EDGE_CURVE ( 'NONE', #9018, #571, #613, .T. ) ;
#4812 = VECTOR ( 'NONE', #1020, 1000.000000000000000 ) ;
#4813 = DIRECTION ( 'NONE',  ( -0.000000000000000000, 1.000000000000000000, -0.000000000000000000 ) ) ;
#4814 = DIRECTION ( 'NONE',  ( -0.000000000000000000, 1.000000000000000000, -0.000000000000000000 ) ) ;
#4815 = CARTESIAN_POINT ( 'NONE',  ( 1.750000000000000000, 0.000000000000000000, 1.599999999999999645 ) ) ;
#4816 = CARTESIAN_POINT ( 'NONE',  ( 19.27821517812503060, 62.76906990284727783, 3.528125000614517059 ) ) ;
#4817 = CIRCLE ( 'NONE', #839, 3.500000000000003109 ) ;
#4818 = DIRECTION ( 'NONE',  ( 0.000000000000000000, 0.000000000000000000, 1.000000000000000000 ) ) ;
#4819 = CARTESIAN_POINT ( 'NONE',  ( 3.556430356250015024, 90.00000000000000000, 3.959375000614517415 ) ) ;
#4820 = ORIENTED_EDGE ( 'NONE', *, *, #1675, .F. ) ;
#4821 =( BOUNDED_CURVE ( )  B_SPLINE_CURVE ( 2, ( #12107, #979, #51, #9158, #2039, #6145, #2172, #8059, #4008, #9225, #8187, #6018, #10014, #3222, #7203, #4070, #183, #11190, #12043, #1109, #1178, #10141, #3157, #7990, #11975, #4979, #5169, #4200, #12174, #2959, #7135, #2243, #6218, #10209, #6939, #3090, #11117, #1246, #1975, #5238, #10986, #7070, #428, #9029, #10924, #11052, #120, #2107, #5101, #3020, #1045 ),
 .UNSPECIFIED., .F., .F. ) 
 B_SPLINE_CURVE_WITH_KNOTS ( ( 3, 2, 2, 2, 2, 2, 2, 2, 2, 2, 2, 2, 2, 2, 2, 2, 2, 2, 2, 2, 2, 2, 2, 2, 2, 3 ),
 ( 0.000000000000000000, 0.03333333333333333287, 0.06666666666666666574, 0.1000000000000000194, 0.1333333333333333315, 0.1666666666666666574, 0.2000000000000000389, 0.2333333333333333648, 0.2666666666666666630, 0.2999999999999999889, 0.3333333333333333148, 0.3666666666666666408, 0.4000000000000000777, 0.4333333333333333481, 0.4666666666666667296, 0.5000000000000000000, 0.5333333333333333259, 0.5666666666666666519, 0.5999999999999999778, 0.6333333333333331927, 0.6666666666666666297, 0.6999999999999999556, 0.7333333333333332815, 0.7666666666666667185, 0.8000000000000001554, 0.8015729473302189989 ),
 .UNSPECIFIED. ) 
 CURVE ( )  GEOMETRIC_REPRESENTATION_ITEM ( )  RATIONAL_B_SPLINE_CURVE ( ( 1.000000000000000000, 0.8660254037844387076, 1.000000000000000000, 0.8660254037844387076, 1.000000000000000000, 0.8660254037844387076, 1.000000000000000000, 0.8660254037844387076, 1.000000000000000000, 0.8660254037844387076, 1.000000000000000000, 0.8660254037844387076, 1.000000000000000000, 0.8660254037844387076, 1.000000000000000000, 0.8660254037844387076, 1.000000000000000000, 0.8660254037844387076, 1.000000000000000000, 0.8660254037844387076, 1.000000000000000000, 0.8660254037844387076, 1.000000000000000000, 0.8660254037844387076, 1.000000000000000000, 0.8660254037844387076, 1.000000000000000000, 0.8660254037844387076, 1.000000000000000000, 0.8660254037844387076, 1.000000000000000000, 0.8660254037844387076, 1.000000000000000000, 0.8660254037844387076, 1.000000000000000000, 0.8660254037844387076, 1.000000000000000000, 0.8660254037844387076, 1.000000000000000000, 0.8660254037844387076, 1.000000000000000000, 0.8660254037844387076, 1.000000000000000000, 0.8660254037844387076, 1.000000000000000000, 0.8660254037844387076, 1.000000000000000000, 0.8660254037844387076, 1.000000000000000000, 0.9936779504969671661, 0.9879525560471726919 ) ) 
 REPRESENTATION_ITEM ( '' )  );
#4822 = PLANE ( 'NONE',  #11640 ) ;
#4823 = ORIENTED_EDGE ( 'NONE', *, *, #440, .F. ) ;
#4824 = DIRECTION ( 'NONE',  ( 0.000000000000000000, 0.000000000000000000, 1.000000000000000000 ) ) ;
#4825 = FACE_BOUND ( 'NONE', #1837, .T. ) ;
#4826 = VECTOR ( 'NONE', #6097, 1000.000000000000000 ) ;
#4827 = CARTESIAN_POINT ( 'NONE',  ( -9.666666666666657193, 79.07477288111861924, -1.000000000000000000 ) ) ;
#4828 = DIRECTION ( 'NONE',  ( 1.000000000000000000, 0.000000000000000000, 0.000000000000000000 ) ) ;
#4829 = ADVANCED_FACE ( 'NONE', ( #6439, #10571 ), #4486, .F. ) ;
#4830 = LINE ( 'NONE', #11888, #5723 ) ;
#4831 = PLANE ( 'NONE',  #11175 ) ;
#4832 = ORIENTED_EDGE ( 'NONE', *, *, #5394, .F. ) ;
#4833 = DIRECTION ( 'NONE',  ( -1.000000000000000000, -0.000000000000000000, -0.000000000000000000 ) ) ;
#4834 = CARTESIAN_POINT ( 'NONE',  ( 34.25000000000000000, 93.41869858279433458, 4.000000000000000000 ) ) ;
#4835 = ORIENTED_EDGE ( 'NONE', *, *, #2335, .F. ) ;
#4836 = DIRECTION ( 'NONE',  ( 0.8660254037844361541, 0.5000000000000042188, -9.389466242107214363E-17 ) ) ;
#4837 = EDGE_LOOP ( 'NONE', ( #6312, #11593, #4902, #10218, #418, #7945, #10787, #6269 ) ) ;
#4838 = VECTOR ( 'NONE', #4007, 1000.000000000000000 ) ;
#4839 = SURFACE_SIDE_STYLE ('',( #8888 ) ) ;
#4840 = EDGE_LOOP ( 'NONE', ( #4234, #5007, #4168, #7450 ) ) ;
#4841 = CYLINDRICAL_SURFACE ( 'NONE', #879, 3.350000000000003642 ) ;
#4842 = LINE ( 'NONE', #8893, #8940 ) ;
#4843 = EDGE_CURVE ( 'NONE', #8608, #4549, #4552, .T. ) ;
#4844 = EDGE_CURVE ( 'NONE', #11182, #1862, #11544, .T. ) ;
#4845 = EDGE_CURVE ( 'NONE', #1436, #6987, #2041, .T. ) ;
#4846 = ORIENTED_EDGE ( 'NONE', *, *, #2587, .F. ) ;
#4847 = AXIS2_PLACEMENT_3D ( 'NONE', #7493, #7182, #12467 ) ;
#4848 = CARTESIAN_POINT ( 'NONE',  ( 45.00000000000000711, 90.00000000000000000, -10.00000000000000000 ) ) ;
#4849 = ORIENTED_EDGE ( 'NONE', *, *, #10959, .F. ) ;
#4850 = LINE ( 'NONE', #3938, #6463 ) ;
#4851 = ORIENTED_EDGE ( 'NONE', *, *, #1699, .F. ) ;
#4852 = CARTESIAN_POINT ( 'NONE',  ( 35.00000000000000000, 126.3079067962035822, 3.340625000614517059 ) ) ;
#4853 = EDGE_LOOP ( 'NONE', ( #5228, #2671, #280, #8620 ) ) ;
#4854 = LINE ( 'NONE', #2105, #12576 ) ;
#4855 = DIRECTION ( 'NONE',  ( -0.000000000000000000, 1.000000000000000000, -0.000000000000000000 ) ) ;
#4856 = AXIS2_PLACEMENT_3D ( 'NONE', #9159, #185, #4202 ) ;
#4857 = CARTESIAN_POINT ( 'NONE',  ( 3.800000000000015365, 108.0133283987163111, 4.175000001229034474 ) ) ;
#4858 = EDGE_CURVE ( 'NONE', #7601, #6408, #1534, .T. ) ;
#4859 = DIRECTION ( 'NONE',  ( 0.000000000000000000, 0.000000000000000000, 1.000000000000000000 ) ) ;
#4860 = ORIENTED_EDGE ( 'NONE', *, *, #10676, .T. ) ;
#4861 = CARTESIAN_POINT ( 'NONE',  ( 50.00000000000000000, 2.000000000000000000, 10.00000000000000000 ) ) ;
#4862 = CARTESIAN_POINT ( 'NONE',  ( 51.63999694657688622, 66.24635823768382181, 1.000000000000003109 ) ) ;
#4863 = CARTESIAN_POINT ( 'NONE',  ( 3.800000000000015365, 90.00000000000000000, 3.200000000000000178 ) ) ;
#4864 = DIRECTION ( 'NONE',  ( -0.000000000000000000, -0.000000000000000000, -1.000000000000000000 ) ) ;
#4865 = ORIENTED_EDGE ( 'NONE', *, *, #8970, .T. ) ;
#4866 = DIRECTION ( 'NONE',  ( -0.9995191440486532741, -0.03100775193798452692, 0.000000000000000000 ) ) ;
#4867 = CARTESIAN_POINT ( 'NONE',  ( 35.00000000000000000, 126.3079067962035822, 3.846875000614517592 ) ) ;
#4868 = ORIENTED_EDGE ( 'NONE', *, *, #8542, .F. ) ;
#4869 = CARTESIAN_POINT ( 'NONE',  ( 35.00000000000000711, 53.97334320256736362, 4.212500000000000355 ) ) ;
#4870 = CYLINDRICAL_SURFACE ( 'NONE', #1201, 1.599999999999993872 ) ;
#4871 = VERTEX_POINT ( 'NONE', #9524 ) ;
#4872 = EDGE_CURVE ( 'NONE', #9364, #8511, #11010, .T. ) ;
#4873 = EDGE_CURVE ( 'NONE', #294, #216, #2464, .T. ) ;
#4874 = CARTESIAN_POINT ( 'NONE',  ( -60.00000000000000000, -6.000000000000000000, 14.99999999999999645 ) ) ;
#4875 = VECTOR ( 'NONE', #9306, 1000.000000000000000 ) ;
#4876 = CARTESIAN_POINT ( 'NONE',  ( 35.00000000000000000, 90.00000000000000000, 5.000000000000000000 ) ) ;
#4877 = DIRECTION ( 'NONE',  ( -0.8660254037844365982, -0.5000000000000036637, 0.000000000000000000 ) ) ;
#4878 = EDGE_CURVE ( 'NONE', #4212, #10011, #9586, .T. ) ;
#4879 = EDGE_CURVE ( 'NONE', #4783, #1668, #2887, .T. ) ;
#4880 = DIRECTION ( 'NONE',  ( 0.000000000000000000, 0.000000000000000000, -1.000000000000000000 ) ) ;
#4881 = CARTESIAN_POINT ( 'NONE',  ( 66.44356964374998142, 108.1539533981018053, 4.221875000614517148 ) ) ;
#4882 = ORIENTED_EDGE ( 'NONE', *, *, #9302, .F. ) ;
#4883 = FACE_OUTER_BOUND ( 'NONE', #3942, .T. ) ;
#4884 = ORIENTED_EDGE ( 'NONE', *, *, #10120, .T. ) ;
#4885 = CIRCLE ( 'NONE', #3645, 2.849999999999999645 ) ;
#4886 = DIRECTION ( 'NONE',  ( 1.000000000000000000, 0.000000000000000000, 0.000000000000000000 ) ) ;
#4887 = AXIS2_PLACEMENT_3D ( 'NONE', #12350, #5538, #2286 ) ;
#4888 = CARTESIAN_POINT ( 'NONE',  ( -48.33333333333332860, 2.000000000000000000, -1.599999999999995426 ) ) ;
#4889 = DIRECTION ( 'NONE',  ( 1.000000000000000000, 0.000000000000000000, 0.000000000000000000 ) ) ;
#4890 = DIRECTION ( 'NONE',  ( -0.000000000000000000, 0.5000000000000000000, 0.8660254037844385966 ) ) ;
#4891 = CARTESIAN_POINT ( 'NONE',  ( 34.49999999999995026, 119.0000000000000000, 0.6666666666666665186 ) ) ;
#4892 = VERTEX_POINT ( 'NONE', #3577 ) ;
#4893 = CIRCLE ( 'NONE', #2613, 30.00000000000000000 ) ;
#4894 = CARTESIAN_POINT ( 'NONE',  ( -6.666666666666660745, 0.000000000000000000, 0.000000000000000000 ) ) ;
#4895 = ITEM_DEFINED_TRANSFORMATION ( 'NONE', 'NONE', #6763,  #5704 ) ;
#4896 = DIRECTION ( 'NONE',  ( 1.000000000000000000, 0.000000000000000000, 0.000000000000000000 ) ) ;
#4897 = CIRCLE ( 'NONE', #2187, 29.99999999999999645 ) ;
#4898 = EDGE_LOOP ( 'NONE', ( #10984, #3879, #10531, #5569 ) ) ;
#4899 = LINE ( 'NONE', #10786, #2433 ) ;
#4900 = ORIENTED_EDGE ( 'NONE', *, *, #4651, .F. ) ;
#4901 = FACE_OUTER_BOUND ( 'NONE', #6011, .T. ) ;
#4902 = ORIENTED_EDGE ( 'NONE', *, *, #271, .F. ) ;
#4903 = EDGE_CURVE ( 'NONE', #7314, #6404, #12699, .T. ) ;
#4904 = LINE ( 'NONE', #3866, #8629 ) ;
#4905 = DIRECTION ( 'NONE',  ( 5.337610695313252124E-17, 0.000000000000000000, -1.000000000000000000 ) ) ;
#4906 = AXIS2_PLACEMENT_3D ( 'NONE', #6688, #5961, #6751 ) ;
#4907 = ORIENTED_EDGE ( 'NONE', *, *, #12433, .F. ) ;
#4908 = DIRECTION ( 'NONE',  ( -0.000000000000000000, 0.000000000000000000, -1.000000000000000000 ) ) ;
#4909 = EDGE_LOOP ( 'NONE', ( #1363, #5983, #8882, #4197, #8934, #1950, #6009, #7083, #11297, #1572, #7471, #543 ) ) ;
#4910 = DIRECTION ( 'NONE',  ( 1.000000000000000000, 0.000000000000000000, 0.000000000000000000 ) ) ;
#4911 = VERTEX_POINT ( 'NONE', #3642 ) ;
#4912 = EDGE_CURVE ( 'NONE', #4450, #12839, #5593, .T. ) ;
#4913 = AXIS2_PLACEMENT_3D ( 'NONE', #12406, #11293, #225 ) ;
#4914 = CARTESIAN_POINT ( 'NONE',  ( 50.72178482187501203, 62.76906990284730625, 4.053125000614517859 ) ) ;
#4915 = VERTEX_POINT ( 'NONE', #12468 ) ;
#4916 = CARTESIAN_POINT ( 'NONE',  ( 3.556430356250015024, 90.00000000000000000, 4.831250000614517148 ) ) ;
#4917 = CARTESIAN_POINT ( 'NONE',  ( 3.800000000000135270, 108.0133283987163679, 3.162500000000000533 ) ) ;
#4918 = EDGE_CURVE ( 'NONE', #10857, #6375, #7622, .T. ) ;
#4919 = CARTESIAN_POINT ( 'NONE',  ( 3.000000000000004441, 27.00000000000000000, -2.500000000000000000 ) ) ;
#4920 = CARTESIAN_POINT ( 'NONE',  ( 3.556430356250028790, 71.84604660189818048, 3.940625000614518036 ) ) ;
#4921 = VECTOR ( 'NONE', #5519, 1000.000000000000114 ) ;
#4922 = PLANE ( 'NONE',  #2076 ) ;
#4923 = ORIENTED_EDGE ( 'NONE', *, *, #3091, .F. ) ;
#4924 = AXIS2_PLACEMENT_3D ( 'NONE', #8417, #9765, #3389 ) ;
#4925 = DIRECTION ( 'NONE',  ( 0.000000000000000000, 0.000000000000000000, 1.000000000000000000 ) ) ;
#4926 = DIRECTION ( 'NONE',  ( 1.000000000000000000, 0.000000000000000000, 0.000000000000000000 ) ) ;
#4927 = ORIENTED_EDGE ( 'NONE', *, *, #6427, .T. ) ;
#4928 = CARTESIAN_POINT ( 'NONE',  ( 0.000000000000000000, 0.000000000000000000, -2.500000000000000000 ) ) ;
#4929 = ORIENTED_EDGE ( 'NONE', *, *, #4236, .T. ) ;
#4930 = ADVANCED_FACE ( 'NONE', ( #7494 ), #9560, .F. ) ;
#4931 =( REPRESENTATION_RELATIONSHIP ('NONE','NONE', #1997, #9523 ) REPRESENTATION_RELATIONSHIP_WITH_TRANSFORMATION ( #9991 )SHAPE_REPRESENTATION_RELATIONSHIP( ) );
#4932 = CARTESIAN_POINT ( 'NONE',  ( 45.00000000000000000, 0.000000000000000000, -7.250000000000000888 ) ) ;
#4933 = AXIS2_PLACEMENT_3D ( 'NONE', #11800, #1988, #5965 ) ;
#4934 = CARTESIAN_POINT ( 'NONE',  ( 3.556430356250014579, 108.1539533981018053, 3.921875000614517326 ) ) ;
#4935 = EDGE_LOOP ( 'NONE', ( #513, #11240, #5997, #1037, #104, #7259, #1083, #10148, #5800, #10980 ) ) ;
#4936 = AXIS2_PLACEMENT_3D ( 'NONE', #1683, #12481, #5669 ) ;
#4937 = CARTESIAN_POINT ( 'NONE',  ( 3.556430356250014579, 108.1539533981018053, 3.921875000614517326 ) ) ;
#4938 = DIRECTION ( 'NONE',  ( 0.000000000000000000, 0.000000000000000000, 1.000000000000000000 ) ) ;
#4939 = DIRECTION ( 'NONE',  ( 0.000000000000000000, -0.000000000000000000, -1.000000000000000000 ) ) ;
#4940 = DIRECTION ( 'NONE',  ( -0.000000000000000000, 0.000000000000000000, 1.000000000000000000 ) ) ;
#4941 = VECTOR ( 'NONE', #11268, 1000.000000000000000 ) ;
#4942 = DIRECTION ( 'NONE',  ( 0.000000000000000000, 0.000000000000000000, 1.000000000000000000 ) ) ;
#4943 = EDGE_CURVE ( 'NONE', #169, #1744, #8098, .T. ) ;
#4944 = CARTESIAN_POINT ( 'NONE',  ( -2.179634403564815859, -5.614030811971695734, -0.8000000000000000444 ) ) ;
#4945 = CARTESIAN_POINT ( 'NONE',  ( 50.72178482187499071, 117.2309300971526937, 4.709375000614516971 ) ) ;
#4946 = ORIENTED_EDGE ( 'NONE', *, *, #9012, .F. ) ;
#4947 = CARTESIAN_POINT ( 'NONE',  ( -4.270088556250601699E-16, 2.000000000000000000, 8.000000000000000000 ) ) ;
#4948 = ORIENTED_EDGE ( 'NONE', *, *, #7104, .F. ) ;
#4949 = CARTESIAN_POINT ( 'NONE',  ( 8.499999999999989342, 69.54849343948980334, -1.000000000000000000 ) ) ;
#4950 = EDGE_CURVE ( 'NONE', #4056, #1497, #1620, .T. ) ;
#4951 = EDGE_CURVE ( 'NONE', #7045, #6408, #6568, .T. ) ;
#4952 = CARTESIAN_POINT ( 'NONE',  ( 1.040000000000000036, 1.154700538379252350, -1.084202172485497162E-16 ) ) ;
#4953 = CARTESIAN_POINT ( 'NONE',  ( 35.00000000000000000, 90.00000000000000000, -8.000000000000000000 ) ) ;
#4954 = DIRECTION ( 'NONE',  ( 0.000000000000000000, 0.000000000000000000, 1.000000000000000000 ) ) ;
#4955 = ORIENTED_EDGE ( 'NONE', *, *, #2926, .T. ) ;
#4956 = CARTESIAN_POINT ( 'NONE',  ( -48.33333333333332860, 0.000000000000000000, -1.500000000000003109 ) ) ;
#4957 = DIRECTION ( 'NONE',  ( 0.000000000000000000, -1.000000000000000000, 0.000000000000000000 ) ) ;
#4958 = VECTOR ( 'NONE', #411, 1000.000000000000000 ) ;
#4959 = EDGE_LOOP ( 'NONE', ( #3986, #7360 ) ) ;
#4960 = ADVANCED_FACE ( 'NONE', ( #10499 ), #2466, .T. ) ;
#4961 = DIRECTION ( 'NONE',  ( -0.000000000000000000, 1.000000000000000000, 0.000000000000000000 ) ) ;
#4962 = EDGE_LOOP ( 'NONE', ( #3543, #11846, #614, #6505, #10600, #8324 ) ) ;
#4963 = VERTEX_POINT ( 'NONE', #8731 ) ;
#4964 = LINE ( 'NONE', #5819, #11751 ) ;
#4965 = CARTESIAN_POINT ( 'NONE',  ( 64.39470308771990403, 100.6987976320522336, 2.708851390588459029 ) ) ;
#4966 = ORIENTED_EDGE ( 'NONE', *, *, #4951, .T. ) ;
#4967 = VECTOR ( 'NONE', #4668, 1000.000000000000000 ) ;
#4968 = VERTEX_POINT ( 'NONE', #12917 ) ;
#4969 = CARTESIAN_POINT ( 'NONE',  ( 1.040000000000000036, 0.000000000000000000, 0.000000000000000000 ) ) ;
#4970 = EDGE_LOOP ( 'NONE', ( #10182, #7587, #1212, #10396 ) ) ;
#4971 = EDGE_CURVE ( 'NONE', #3204, #8770, #4809, .T. ) ;
#4972 = FACE_OUTER_BOUND ( 'NONE', #2548, .T. ) ;
#4973 = EDGE_LOOP ( 'NONE', ( #8310, #3270, #3131, #6871 ) ) ;
#4974 = CARTESIAN_POINT ( 'NONE',  ( 50.72178482187499071, 117.2309300971526937, 4.653125000614517504 ) ) ;
#4975 = AXIS2_PLACEMENT_3D ( 'NONE', #12803, #5804, #9795 ) ;
#4976 = ORIENTED_EDGE ( 'NONE', *, *, #4986, .F. ) ;
#4977 = AXIS2_PLACEMENT_3D ( 'NONE', #11301, #1356, #432 ) ;
#4978 = LINE ( 'NONE', #6017, #11087 ) ;
#4979 = CARTESIAN_POINT ( 'NONE',  ( 3.556430356250014579, 108.1539533981018053, 3.865625000614517415 ) ) ;
#4980 = CARTESIAN_POINT ( 'NONE',  ( 19.40000000000002700, 62.98000740192551206, 3.387500001229033941 ) ) ;
#4981 = EDGE_CURVE ( 'NONE', #1892, #1472, #8725, .T. ) ;
#4982 = CARTESIAN_POINT ( 'NONE',  ( -43.33333333333332860, 41.93190556325238560, -1.000000000000001110 ) ) ;
#4983 = AXIS2_PLACEMENT_3D ( 'NONE', #2239, #1434, #8119 ) ;
#4984 = VERTEX_POINT ( 'NONE', #1927 ) ;
#4985 = CARTESIAN_POINT ( 'NONE',  ( 50.59999999999999432, 117.0199925980744666, 4.850000000000000533 ) ) ;
#4986 = EDGE_CURVE ( 'NONE', #5993, #8371, #11994, .T. ) ;
#4987 = PLANE ( 'NONE',  #8343 ) ;
#4988 = CARTESIAN_POINT ( 'NONE',  ( -18.33333333333332504, 46.12451549659709116, 7.999999999999996447 ) ) ;
#4989 = VERTEX_POINT ( 'NONE', #6827 ) ;
#4990 = CARTESIAN_POINT ( 'NONE',  ( 48.49999999999995737, 86.00000000000000000, -10.00000000000000000 ) ) ;
#4991 = VERTEX_POINT ( 'NONE', #3964 ) ;
#4992 = CIRCLE ( 'NONE', #1012, 3.500000000000003109 ) ;
#4993 = DIRECTION ( 'NONE',  ( -1.000000000000000000, 9.570888143320317860E-16, 0.000000000000000000 ) ) ;
#4994 = UNCERTAINTY_MEASURE_WITH_UNIT (LENGTH_MEASURE( 1.000000000000000082E-05 ), #3069, 'distance_accuracy_value', 'NONE');
#4995 = CARTESIAN_POINT ( 'NONE',  ( 66.44356964374999563, 90.00000000000000000, 4.128125000614517148 ) ) ;
#4996 = ORIENTED_EDGE ( 'NONE', *, *, #8402, .F. ) ;
#4997 = AXIS2_PLACEMENT_3D ( 'NONE', #5043, #2045, #5174 ) ;
#4998 = PLANE ( 'NONE',  #11436 ) ;
#4999 = ADVANCED_FACE ( 'NONE', ( #9901 ), #4998, .T. ) ;
#5000 = AXIS2_PLACEMENT_3D ( 'NONE', #905, #7855, #4910 ) ;
#5001 = CARTESIAN_POINT ( 'NONE',  ( 1.040000000000000036, 0.000000000000000000, 1.000000000000000000 ) ) ;
#5002 = EDGE_CURVE ( 'NONE', #3280, #5034, #7881, .T. ) ;
#5003 = CYLINDRICAL_SURFACE ( 'NONE', #2184, 30.19999999999998863 ) ;
#5004 = CARTESIAN_POINT ( 'NONE',  ( 31.99902028769960438, 88.51116798584881451, -3.800000000000000266 ) ) ;
#5005 = DIRECTION ( 'NONE',  ( 1.000000000000000000, 0.000000000000000000, 0.000000000000000000 ) ) ;
#5006 = CARTESIAN_POINT ( 'NONE',  ( 3.556430356250015024, 90.00000000000000000, 4.409375000614517148 ) ) ;
#5007 = ORIENTED_EDGE ( 'NONE', *, *, #11742, .F. ) ;
#5008 = VECTOR ( 'NONE', #10116, 1000.000000000000000 ) ;
#5009 = DIRECTION ( 'NONE',  ( 0.1305261922200528224, 0.9914448613738103822, -0.000000000000000000 ) ) ;
#5010 = EDGE_LOOP ( 'NONE', ( #6873, #6864, #12485, #9083 ) ) ;
#5011 = EDGE_CURVE ( 'NONE', #7582, #11451, #5798, .T. ) ;
#5012 = CARTESIAN_POINT ( 'NONE',  ( 35.00000000000000000, 126.0266567974326222, 3.537499999999999645 ) ) ;
#5013 = CARTESIAN_POINT ( 'NONE',  ( 40.00000000000000000, 2.000000000000000000, 10.00000000000000000 ) ) ;
#5014 = DIRECTION ( 'NONE',  ( -1.000000000000000000, -0.000000000000000000, -0.000000000000000000 ) ) ;
#5015 = AXIS2_PLACEMENT_3D ( 'NONE', #11684, #4818, #8804 ) ;
#5016 = ADVANCED_FACE ( 'NONE', ( #6 ), #805, .F. ) ;
#5017 = ORIENTED_EDGE ( 'NONE', *, *, #3260, .F. ) ;
#5018 = VECTOR ( 'NONE', #4543, 1000.000000000000000 ) ;
#5019 = CARTESIAN_POINT ( 'NONE',  ( 7.264852530253062213, 98.48596457872582732, 4.000000000000000000 ) ) ;
#5020 = DIRECTION ( 'NONE',  ( 0.000000000000000000, 0.000000000000000000, -1.000000000000000000 ) ) ;
#5021 = ORIENTED_EDGE ( 'NONE', *, *, #12102, .T. ) ;
#5022 = ORIENTED_EDGE ( 'NONE', *, *, #301, .F. ) ;
#5023 = EDGE_CURVE ( 'NONE', #11514, #29, #980, .T. ) ;
#5024 = PLANE ( 'NONE',  #11944 ) ;
#5025 = ORIENTED_EDGE ( 'NONE', *, *, #7115, .T. ) ;
#5026 = CARTESIAN_POINT ( 'NONE',  ( -62.98205080756885366, 29.16506350946109194, 0.000000000000000000 ) ) ;
#5027 = AXIS2_PLACEMENT_3D ( 'NONE', #69, #10028, #7021 ) ;
#5028 = CARTESIAN_POINT ( 'NONE',  ( 30.00000000000000711, 0.000000000000000000, 1.500000000000000666 ) ) ;
#5029 = ORIENTED_EDGE ( 'NONE', *, *, #5954, .T. ) ;
#5030 = ORIENTED_EDGE ( 'NONE', *, *, #9280, .T. ) ;
#5031 = CARTESIAN_POINT ( 'NONE',  ( 7.500000000000000000, 27.00000000000000000, 1.599999999999992095 ) ) ;
#5032 = VERTEX_POINT ( 'NONE', #2786 ) ;
#5033 = CARTESIAN_POINT ( 'NONE',  ( 3.556430356250014579, 108.1539533981018053, 3.415625000614517237 ) ) ;
#5034 = VERTEX_POINT ( 'NONE', #3901 ) ;
#5035 = CONICAL_SURFACE ( 'NONE', #9219, 1732.050807568857181, 1.047197551196592746 ) ;
#5036 = CYLINDRICAL_SURFACE ( 'NONE', #10927, 1.599999999999992095 ) ;
#5037 = EDGE_CURVE ( 'NONE', #10351, #2190, #4340, .T. ) ;
#5038 = ORIENTED_EDGE ( 'NONE', *, *, #6229, .F. ) ;
#5039 = EDGE_CURVE ( 'NONE', #8420, #193, #6073, .T. ) ;
#5040 = CARTESIAN_POINT ( 'NONE',  ( 0.000000000000000000, 3.490243377569956061E-16, -2.849999999999999645 ) ) ;
#5041 = CARTESIAN_POINT ( 'NONE',  ( -48.33333333333332860, -5.000000000000000000, 1.499999999999999556 ) ) ;
#5042 = FACE_OUTER_BOUND ( 'NONE', #8316, .T. ) ;
#5043 = CARTESIAN_POINT ( 'NONE',  ( 1.040000000000000036, 0.5773502691896263972, -1.000000000000000000 ) ) ;
#5044 = EDGE_LOOP ( 'NONE', ( #7375, #2638, #9922, #4263, #8890, #2233 ) ) ;
#5045 = CARTESIAN_POINT ( 'NONE',  ( 3.800000000000015365, 108.0133283987163111, 3.162500000000000533 ) ) ;
#5046 = LINE ( 'NONE', #12718, #3135 ) ;
#5047 = CARTESIAN_POINT ( 'NONE',  ( 45.00000000000000000, 2.000000000000001332, -7.349999999999989875 ) ) ;
#5048 = ORIENTED_EDGE ( 'NONE', *, *, #8911, .T. ) ;
#5049 = DIRECTION ( 'NONE',  ( -0.7071067811865489050, 8.659560562354915602E-17, -0.7071067811865462405 ) ) ;
#5050 = EDGE_LOOP ( 'NONE', ( #553, #8460, #4712, #3531 ) ) ;
#5051 =( GEOMETRIC_REPRESENTATION_CONTEXT ( 3 ) GLOBAL_UNCERTAINTY_ASSIGNED_CONTEXT ( ( #11450 ) ) GLOBAL_UNIT_ASSIGNED_CONTEXT ( ( #11723, #4604, #8717 ) ) REPRESENTATION_CONTEXT ( 'NONE', 'WORKASPACE' ) );
#5052 = DIRECTION ( 'NONE',  ( 0.000000000000000000, 0.000000000000000000, 1.000000000000000000 ) ) ;
#5053 = CARTESIAN_POINT ( 'NONE',  ( -53.33333333333332149, 33.84900179459754810, -0.9999999999999997780 ) ) ;
#5054 = ORIENTED_EDGE ( 'NONE', *, *, #8525, .T. ) ;
#5055 = CARTESIAN_POINT ( 'NONE',  ( 19.27821517812500574, 117.2309300971526937, 3.434375000614517059 ) ) ;
#5056 = LINE ( 'NONE', #8144, #12066 ) ;
#5057 = EDGE_CURVE ( 'NONE', #3989, #6204, #11869, .T. ) ;
#5058 = CARTESIAN_POINT ( 'NONE',  ( 35.00000000000000000, 90.00000000000000000, -3.000000000000000000 ) ) ;
#5059 = AXIS2_PLACEMENT_3D ( 'NONE', #6650, #4440, #5612 ) ;
#5060 = PLANE ( 'NONE',  #4705 ) ;
#5061 = LINE ( 'NONE', #79, #11368 ) ;
#5062 = DIRECTION ( 'NONE',  ( 0.000000000000000000, 0.000000000000000000, 1.000000000000000000 ) ) ;
#5063 = EDGE_CURVE ( 'NONE', #681, #6762, #869, .T. ) ;
#5064 = DIRECTION ( 'NONE',  ( 0.000000000000000000, 1.000000000000000000, 0.000000000000000000 ) ) ;
#5065 = CARTESIAN_POINT ( 'NONE',  ( 66.44356964375000985, 71.84604660189820891, 3.246875000614517504 ) ) ;
#5066 = VERTEX_POINT ( 'NONE', #3832 ) ;
#5067 = EDGE_CURVE ( 'NONE', #9866, #7702, #7048, .T. ) ;
#5068 = CARTESIAN_POINT ( 'NONE',  ( -6.666666666666660745, -5.000000000000000000, -1.499999999999999556 ) ) ;
#5069 = VERTEX_POINT ( 'NONE', #5849 ) ;
#5070 = ADVANCED_FACE ( 'NONE', ( #1865 ), #4870, .F. ) ;
#5071 = SURFACE_SIDE_STYLE ('',( #1078 ) ) ;
#5072 = AXIS2_PLACEMENT_3D ( 'NONE', #1258, #6292, #10155 ) ;
#5073 = DIRECTION ( 'NONE',  ( -1.000000000000000000, 0.000000000000000000, 0.000000000000000000 ) ) ;
#5074 = CARTESIAN_POINT ( 'NONE',  ( 33.50000000000000711, 67.79999999999999716, 8.000000000000000000 ) ) ;
#5075 = DIRECTION ( 'NONE',  ( 5.337610695313252124E-17, 0.000000000000000000, -1.000000000000000000 ) ) ;
#5076 = VERTEX_POINT ( 'NONE', #1064 ) ;
#5077 = CARTESIAN_POINT ( 'NONE',  ( -43.33333333333332860, 79.07477288111861924, -1.000000000000001110 ) ) ;
#5078 = CARTESIAN_POINT ( 'NONE',  ( 3.800000000000001155, 108.0133283987163111, 4.175000001229035362 ) ) ;
#5079 = EDGE_LOOP ( 'NONE', ( #2395, #3486, #7111, #2465 ) ) ;
#5080 = CARTESIAN_POINT ( 'NONE',  ( 35.00000000000000000, 90.00000000000000000, 1.000000000000003109 ) ) ;
#5081 = ORIENTED_EDGE ( 'NONE', *, *, #149, .F. ) ;
#5082 = EDGE_CURVE ( 'NONE', #5372, #237, #5056, .T. ) ;
#5083 = SURFACE_STYLE_USAGE ( .BOTH. , #1159 ) ;
#5084 = ORIENTED_EDGE ( 'NONE', *, *, #2430, .F. ) ;
#5085 = FACE_BOUND ( 'NONE', #4081, .T. ) ;
#5086 = AXIS2_PLACEMENT_3D ( 'NONE', #12480, #11232, #11424 ) ;
#5087 = DIRECTION ( 'NONE',  ( -0.000000000000000000, -0.000000000000000000, -1.000000000000000000 ) ) ;
#5088 = ORIENTED_EDGE ( 'NONE', *, *, #8326, .T. ) ;
#5089 = VECTOR ( 'NONE', #10713, 1000.000000000000000 ) ;
#5090 = ORIENTED_EDGE ( 'NONE', *, *, #10556, .F. ) ;
#5091 = AXIS2_PLACEMENT_3D ( 'NONE', #7752, #8, #10825 ) ;
#5092 = DIRECTION ( 'NONE',  ( -1.000000000000000000, 0.000000000000000000, 0.000000000000000000 ) ) ;
#5093 = ORIENTED_EDGE ( 'NONE', *, *, #8064, .F. ) ;
#5094 = SHAPE_DEFINITION_REPRESENTATION ( #9501, #9014 ) ;
#5095 = CARTESIAN_POINT ( 'NONE',  ( 66.44356964374998142, 108.1539533981018053, 4.165625000614516793 ) ) ;
#5096 = ORIENTED_EDGE ( 'NONE', *, *, #9242, .F. ) ;
#5097 = PLANE ( 'NONE',  #5495 ) ;
#5098 = ORIENTED_EDGE ( 'NONE', *, *, #6379, .T. ) ;
#5099 = ADVANCED_FACE ( 'NONE', ( #7153 ), #4221, .F. ) ;
#5100 = DIRECTION ( 'NONE',  ( 0.000000000000000000, -1.000000000000000000, 0.000000000000000000 ) ) ;
#5101 = CARTESIAN_POINT ( 'NONE',  ( 3.556430356250015024, 90.00000000000000000, 3.003125000614517148 ) ) ;
#5102 = AXIS2_PLACEMENT_3D ( 'NONE', #11604, #10363, #1396 ) ;
#5103 = CARTESIAN_POINT ( 'NONE',  ( -38.66666666666665719, 46.12451549659709116, -7.999999999999996447 ) ) ;
#5104 = CARTESIAN_POINT ( 'NONE',  ( 66.19999999999997442, 108.0133283987163253, 3.575000001229033941 ) ) ;
#5105 = DIRECTION ( 'NONE',  ( 0.000000000000000000, 0.000000000000000000, 1.000000000000000000 ) ) ;
#5106 = EDGE_CURVE ( 'NONE', #85, #1209, #7475, .T. ) ;
#5108 = EDGE_CURVE ( 'NONE', #9462, #5352, #8078, .T. ) ;
#5107 = ORIENTED_EDGE ( 'NONE', *, *, #7675, .T. ) ;
#5109 = CARTESIAN_POINT ( 'NONE',  ( 3.556430356250014579, 108.1539533981018053, 4.821875000614516793 ) ) ;
#5110 = CIRCLE ( 'NONE', #83, 1.599999999999990319 ) ;
#5111 = CARTESIAN_POINT ( 'NONE',  ( 3.000000000000002665, 30.00000000000000000, 8.000000000000000000 ) ) ;
#5112 = CARTESIAN_POINT ( 'NONE',  ( 44.60848457269055700, 119.8079162999732432, 3.000000000000003109 ) ) ;
#5113 = ORIENTED_EDGE ( 'NONE', *, *, #1198, .F. ) ;
#5114 = VECTOR ( 'NONE', #11306, 1000.000000000000000 ) ;
#5115 = CARTESIAN_POINT ( 'NONE',  ( 35.00000000000000000, 90.00000000000000000, -3.799999999999999822 ) ) ;
#5116 = ORIENTED_EDGE ( 'NONE', *, *, #12486, .T. ) ;
#5117 = PLANE ( 'NONE',  #5657 ) ;
#5118 = EDGE_CURVE ( 'NONE', #6806, #376, #6219, .T. ) ;
#5119 = CARTESIAN_POINT ( 'NONE',  ( 3.556430356250015024, 90.00000000000000000, 3.453125000614517770 ) ) ;
#5120 = VERTEX_POINT ( 'NONE', #10162 ) ;
#5121 = CARTESIAN_POINT ( 'NONE',  ( 50.72178482187501203, 62.76906990284730625, 3.659375000614517592 ) ) ;
#5122 = DIRECTION ( 'NONE',  ( 0.000000000000000000, -1.000000000000000000, -0.000000000000000000 ) ) ;
#5123 = AXIS2_PLACEMENT_3D ( 'NONE', #8096, #7905, #12084 ) ;
#5124 = DIRECTION ( 'NONE',  ( 1.000000000000000000, 0.000000000000000000, 0.000000000000000000 ) ) ;
#5125 =( NAMED_UNIT ( * ) SI_UNIT ( $, .STERADIAN. ) SOLID_ANGLE_UNIT ( ) );
#5126 = PRODUCT_RELATED_PRODUCT_CATEGORY ( 'part', '', ( #8459 ) ) ;
#5127 = DIRECTION ( 'NONE',  ( 0.000000000000000000, -1.000000000000000000, 0.000000000000000000 ) ) ;
#5128 = CARTESIAN_POINT ( 'NONE',  ( 45.00000000000000000, 0.000000000000000000, 4.150000000000003908 ) ) ;
#5129 = CIRCLE ( 'NONE', #8486, 3.351416843938785028 ) ;
#5130 = FACE_OUTER_BOUND ( 'NONE', #7453, .T. ) ;
#5131 = EDGE_CURVE ( 'NONE', #2970, #8362, #7286, .T. ) ;
#5132 = MECHANICAL_DESIGN_GEOMETRIC_PRESENTATION_REPRESENTATION (  '', ( #3052 ), #6173 ) ;
#5133 = DIRECTION ( 'NONE',  ( -1.000000000000000000, 0.000000000000000000, 0.000000000000000000 ) ) ;
#5134 = CARTESIAN_POINT ( 'NONE',  ( 3.556430356250014579, 103.6582747873649311, 3.031161570002773420 ) ) ;
#5135 = ORIENTED_EDGE ( 'NONE', *, *, #12357, .T. ) ;
#5136 = LINE ( 'NONE', #11220, #7876 ) ;
#5137 = VERTEX_POINT ( 'NONE', #7092 ) ;
#5138 = AXIS2_PLACEMENT_3D ( 'NONE', #3654, #10583, #686 ) ;
#5139 = DIRECTION ( 'NONE',  ( 0.000000000000000000, 0.000000000000000000, 1.000000000000000000 ) ) ;
#5141 = EDGE_CURVE ( 'NONE', #3861, #4333, #7884, .T. ) ;
#5140 = CARTESIAN_POINT ( 'NONE',  ( 17.54971918633085437, 66.83239978927272773, -1.000000000000000000 ) ) ;
#5142 = CARTESIAN_POINT ( 'NONE',  ( 17.55231228847961944, 66.83584248194507893, 3.000000000000000888 ) ) ;
#5143 = EDGE_LOOP ( 'NONE', ( #10082, #1369, #5181, #1354 ) ) ;
#5144 = DIRECTION ( 'NONE',  ( -0.000000000000000000, -0.000000000000000000, 1.000000000000000000 ) ) ;
#5145 = EDGE_CURVE ( 'NONE', #4056, #5747, #3243, .T. ) ;
#5146 = CARTESIAN_POINT ( 'NONE',  ( 35.00000000000000000, 90.00000000000000000, 4.000000000000000000 ) ) ;
#5147 = EDGE_LOOP ( 'NONE', ( #7533, #4378, #9977 ) ) ;
#5148 =( LENGTH_UNIT ( ) NAMED_UNIT ( * ) SI_UNIT ( .MILLI., .METRE. ) );
#5149 = VERTEX_POINT ( 'NONE', #10291 ) ;
#5150 = TOROIDAL_SURFACE ( 'NONE', #10587, 1.599999999999999645, 0.1000000000000000056 ) ;
#5151 = PRESENTATION_STYLE_ASSIGNMENT (( #5083 ) ) ;
#5152 = EDGE_LOOP ( 'NONE', ( #566, #3690, #5616, #9270, #2542, #10983 ) ) ;
#5153 = FACE_OUTER_BOUND ( 'NONE', #5959, .T. ) ;
#5154 = PLANE ( 'NONE',  #12716 ) ;
#5155 = ORIENTED_EDGE ( 'NONE', *, *, #12796, .T. ) ;
#5156 = ADVANCED_FACE ( 'NONE', ( #7026 ), #6039, .F. ) ;
#5157 = ORIENTED_EDGE ( 'NONE', *, *, #1272, .F. ) ;
#5158 = VECTOR ( 'NONE', #9915, 1000.000000000000000 ) ;
#5159 = LINE ( 'NONE', #4382, #306 ) ;
#5160 = ORIENTED_EDGE ( 'NONE', *, *, #5039, .T. ) ;
#5161 = EDGE_CURVE ( 'NONE', #3039, #946, #5190, .T. ) ;
#5162 = APPLICATION_PROTOCOL_DEFINITION ( 'draft international standard', 'automotive_design', 1998, #1838 ) ;
#5163 = CARTESIAN_POINT ( 'NONE',  ( 50.72178482187499071, 117.2309300971526937, 4.653125000614517504 ) ) ;
#5164 = ORIENTED_EDGE ( 'NONE', *, *, #10221, .F. ) ;
#5165 = CYLINDRICAL_SURFACE ( 'NONE', #6747, 3.350000000000000089 ) ;
#5166 = DIRECTION ( 'NONE',  ( 0.000000000000000000, 0.000000000000000000, -1.000000000000000000 ) ) ;
#5167 = ORIENTED_EDGE ( 'NONE', *, *, #388, .F. ) ;
#5168 = LINE ( 'NONE', #2171, #9845 ) ;
#5169 = CARTESIAN_POINT ( 'NONE',  ( 19.27821517812500574, 117.2309300971526937, 3.828125000614516882 ) ) ;
#5170 = AXIS2_PLACEMENT_3D ( 'NONE', #11414, #5457, #9452 ) ;
#5171 = PLANE ( 'NONE',  #4856 ) ;
#5172 = LINE ( 'NONE', #8061, #1210 ) ;
#5173 =( NAMED_UNIT ( * ) PLANE_ANGLE_UNIT ( ) SI_UNIT ( $, .RADIAN. ) );
#5174 = DIRECTION ( 'NONE',  ( 1.000000000000000000, 0.000000000000000000, -0.000000000000000000 ) ) ;
#5175 = ADVANCED_FACE ( 'NONE', ( #1128 ), #9179, .F. ) ;
#5176 = EDGE_LOOP ( 'NONE', ( #2354, #8870, #445, #2358 ) ) ;
#5177 = CARTESIAN_POINT ( 'NONE',  ( 3.800000000000025135, 71.98667160128366049, 3.687500000000000888 ) ) ;
#5178 = ORIENTED_EDGE ( 'NONE', *, *, #11742, .T. ) ;
#5179 = VECTOR ( 'NONE', #153, 1000.000000000000000 ) ;
#5180 = CARTESIAN_POINT ( 'NONE',  ( 1.269999999999999796, -2.850000000000002753, -3.490243377569956061E-16 ) ) ;
#5181 = ORIENTED_EDGE ( 'NONE', *, *, #10833, .T. ) ;
#5182 = CARTESIAN_POINT ( 'NONE',  ( 0.1698013801012111523, -5.473461295629626022, 0.000000000000000000 ) ) ;
#5183 = EDGE_LOOP ( 'NONE', ( #2913, #10859, #11100, #6574 ) ) ;
#5184 = DIRECTION ( 'NONE',  ( 0.000000000000000000, -0.000000000000000000, 1.000000000000000000 ) ) ;
#5185 = B_SPLINE_CURVE_WITH_KNOTS ( 'NONE', 3,
 ( #11797, #1855, #858, #4862 ),
 .UNSPECIFIED., .F., .F.,
 ( 4, 4 ),
 ( 0.000000000000000000, 0.5999999999999994227 ),
 .UNSPECIFIED. ) ;
#5186 = CARTESIAN_POINT ( 'NONE',  ( 19.27821517812503060, 62.76906990284727783, 4.428125000614516971 ) ) ;
#5187 = ORIENTED_EDGE ( 'NONE', *, *, #9714, .T. ) ;
#5188 = EDGE_CURVE ( 'NONE', #7039, #2334, #5319, .T. ) ;
#5189 = CARTESIAN_POINT ( 'NONE',  ( 3.556430356250015024, 90.00000000000000000, 4.859375000614517326 ) ) ;
#5190 = LINE ( 'NONE', #6101, #148 ) ;
#5192 = AXIS2_PLACEMENT_3D ( 'NONE', #8044, #5087, #107 ) ;
#5191 = PLANE ( 'NONE',  #2702 ) ;
#5193 = CARTESIAN_POINT ( 'NONE',  ( 66.19999999999998863, 90.00000000000000000, 3.987500001229034030 ) ) ;
#5194 = ADVANCED_FACE ( 'NONE', ( #2059 ), #2192, .T. ) ;
#5195 = CARTESIAN_POINT ( 'NONE',  ( 31.86869970978804290, 88.80942934165229019, 4.000000000000000000 ) ) ;
#5196 = CARTESIAN_POINT ( 'NONE',  ( 66.19999999999998863, 90.00000000000000000, 5.000000000000000000 ) ) ;
#5197 = CARTESIAN_POINT ( 'NONE',  ( 49.99999999999996447, 90.00000000000000000, -8.000000000000000000 ) ) ;
#5198 = VECTOR ( 'NONE', #1243, 1000.000000000000000 ) ;
#5199 = DIRECTION ( 'NONE',  ( 0.000000000000000000, 0.000000000000000000, -1.000000000000000000 ) ) ;
#5200 = CARTESIAN_POINT ( 'NONE',  ( -3.666666666666659413, 79.07477288111861924, 0.9999999999999991118 ) ) ;
#5201 = EDGE_LOOP ( 'NONE', ( #3199, #7911, #2111, #10283 ) ) ;
#5202 = EDGE_CURVE ( 'NONE', #11262, #11476, #7482, .T. ) ;
#5203 = CARTESIAN_POINT ( 'NONE',  ( 35.00000000000000000, 90.00000000000000000, -1.000000000000000888 ) ) ;
#5204 = VERTEX_POINT ( 'NONE', #10229 ) ;
#5205 = CARTESIAN_POINT ( 'NONE',  ( 7.499999999999992895, 25.35000000000000497, 0.000000000000000000 ) ) ;
#5206 = AXIS2_PLACEMENT_3D ( 'NONE', #11523, #2568, #845 ) ;
#5207 = AXIS2_PLACEMENT_3D ( 'NONE', #5380, #7546, #4607 ) ;
#5208 = DIRECTION ( 'NONE',  ( -0.5877852522924753575, 0.8090169943749458970, 0.000000000000000000 ) ) ;
#5209 = DIRECTION ( 'NONE',  ( -0.000000000000000000, -0.000000000000000000, -1.000000000000000000 ) ) ;
#5210 = CARTESIAN_POINT ( 'NONE',  ( 30.00000000000000711, 0.000000000000000000, 10.00000000000000000 ) ) ;
#5211 = ORIENTED_EDGE ( 'NONE', *, *, #4872, .F. ) ;
#5212 = DIRECTION ( 'NONE',  ( 0.000000000000000000, 0.000000000000000000, -1.000000000000000000 ) ) ;
#5213 = DIRECTION ( 'NONE',  ( 0.000000000000000000, 0.000000000000000000, 1.000000000000000000 ) ) ;
#5214 = ORIENTED_EDGE ( 'NONE', *, *, #9357, .F. ) ;
#5215 = VECTOR ( 'NONE', #3620, 1000.000000000000000 ) ;
#5216 = DIRECTION ( 'NONE',  ( 0.9510565162951543083, -0.3090169943749451198, 0.000000000000000000 ) ) ;
#5217 = ORIENTED_EDGE ( 'NONE', *, *, #4845, .F. ) ;
#5218 = PRODUCT_RELATED_PRODUCT_CATEGORY ( 'part', '', ( #1451 ) ) ;
#5219 = LINE ( 'NONE', #2153, #6304 ) ;
#5220 = ORIENTED_EDGE ( 'NONE', *, *, #7869, .T. ) ;
#5221 = CARTESIAN_POINT ( 'NONE',  ( 35.00000000000000000, 90.00000000000000000, -3.799999999999999378 ) ) ;
#5222 = CARTESIAN_POINT ( 'NONE',  ( 25.00000000000000355, 2.000000000000000000, 5.750000000000000000 ) ) ;
#5223 = EDGE_CURVE ( 'NONE', #242, #4728, #2263, .T. ) ;
#5224 = EDGE_LOOP ( 'NONE', ( #2892, #8948 ) ) ;
#5225 = VECTOR ( 'NONE', #5607, 1000.000000000000000 ) ;
#5226 = ORIENTED_EDGE ( 'NONE', *, *, #12643, .T. ) ;
#5227 = DIRECTION ( 'NONE',  ( -0.000000000000000000, 1.000000000000000000, -0.000000000000000000 ) ) ;
#5228 = ORIENTED_EDGE ( 'NONE', *, *, #4508, .F. ) ;
#5229 = SHAPE_DEFINITION_REPRESENTATION ( #12317, #11692 ) ;
#5230 = CARTESIAN_POINT ( 'NONE',  ( 3.556430356250028790, 71.84604660189818048, 3.940625000614518036 ) ) ;
#5231 = ORIENTED_EDGE ( 'NONE', *, *, #364, .F. ) ;
#5232 = CARTESIAN_POINT ( 'NONE',  ( 0.000000000000000000, 0.000000000000000000, -0.8000000000000000444 ) ) ;
#5233 = PRODUCT_DEFINITION_SHAPE ( 'NONE', 'NONE',  #12968 ) ;
#5234 = DIRECTION ( 'NONE',  ( 0.4719909656437444867, -0.8816033849473842166, 0.000000000000000000 ) ) ;
#5235 = ORIENTED_EDGE ( 'NONE', *, *, #3128, .F. ) ;
#5236 = CIRCLE ( 'NONE', #6687, 31.20000000000000639 ) ;
#5237 = DIRECTION ( 'NONE',  ( -0.8660254037844361541, -0.5000000000000042188, -9.389466242107216828E-17 ) ) ;
#5238 = CARTESIAN_POINT ( 'NONE',  ( 35.00000000000000000, 126.3079067962036106, 3.340625000614517504 ) ) ;
#5239 = EDGE_CURVE ( 'NONE', #11653, #376, #266, .T. ) ;
#5240 = CARTESIAN_POINT ( 'NONE',  ( 31.80092274341787828, 89.00581455129388075, 4.000000000000000000 ) ) ;
#5241 = CARTESIAN_POINT ( 'NONE',  ( 35.49999999999995026, 118.9978446673979704, 1.000000000000003109 ) ) ;
#5242 = EDGE_CURVE ( 'NONE', #3935, #5315, #11271, .T. ) ;
#5243 = DIRECTION ( 'NONE',  ( 0.000000000000000000, 0.000000000000000000, 1.000000000000000000 ) ) ;
#5244 = ORIENTED_EDGE ( 'NONE', *, *, #3629, .T. ) ;
#5245 = AXIS2_PLACEMENT_3D ( 'NONE', #8593, #11720, #1781 ) ;
#5246 = CARTESIAN_POINT ( 'NONE',  ( 3.800000000000015365, 108.0133283987163111, 4.062500000000000000 ) ) ;
#5247 = ORIENTED_EDGE ( 'NONE', *, *, #4844, .T. ) ;
#5248 = DIRECTION ( 'NONE',  ( 1.000000000000000000, 0.000000000000000000, 0.000000000000000000 ) ) ;
#5249 = ORIENTED_EDGE ( 'NONE', *, *, #10868, .T. ) ;
#5250 = CARTESIAN_POINT ( 'NONE',  ( 7.369500000000001272, 0.000000000000000000, 0.000000000000000000 ) ) ;
#5251 = VERTEX_POINT ( 'NONE', #5578 ) ;
#5252 = DIRECTION ( 'NONE',  ( 0.000000000000000000, -0.8660254037844384856, -0.5000000000000003331 ) ) ;
#5253 = CARTESIAN_POINT ( 'NONE',  ( 19.27821517812503060, 62.76906990284727783, 3.078125000614517326 ) ) ;
#5254 = EDGE_CURVE ( 'NONE', #6459, #835, #10422, .T. ) ;
#5255 = CARTESIAN_POINT ( 'NONE',  ( 3.556430356250014579, 108.1539533981018053, 4.371875000614516615 ) ) ;
#5256 = AXIS2_PLACEMENT_3D ( 'NONE', #9949, #12042, #3089 ) ;
#5257 = DIRECTION ( 'NONE',  ( 0.000000000000000000, 0.000000000000000000, 1.000000000000000000 ) ) ;
#5258 = LINE ( 'NONE', #4284, #11885 ) ;
#5259 = DIRECTION ( 'NONE',  ( -1.000000000000000000, 0.000000000000000000, 0.000000000000000000 ) ) ;
#5260 = DIRECTION ( 'NONE',  ( 0.000000000000000000, 1.000000000000000000, 0.000000000000000000 ) ) ;
#5261 = AXIS2_PLACEMENT_3D ( 'NONE', #9808, #35, #4052 ) ;
#5262 = DIRECTION ( 'NONE',  ( -0.000000000000000000, -1.000000000000000000, -0.000000000000000000 ) ) ;
#5263 = CARTESIAN_POINT ( 'NONE',  ( 35.00000000000000000, 90.00000000000000000, 6.000000000000000000 ) ) ;
#5264 = DIRECTION ( 'NONE',  ( 0.000000000000000000, 0.000000000000000000, 1.000000000000000000 ) ) ;
#5265 = ORIENTED_EDGE ( 'NONE', *, *, #6068, .T. ) ;
#5266 = EDGE_CURVE ( 'NONE', #7601, #11985, #12453, .T. ) ;
#5267 = CYLINDRICAL_SURFACE ( 'NONE', #7465, 1.599999999999990319 ) ;
#5268 = ORIENTED_EDGE ( 'NONE', *, *, #5678, .F. ) ;
#5269 = DIRECTION ( 'NONE',  ( 0.000000000000000000, 0.000000000000000000, 1.000000000000000000 ) ) ;
#5270 = DIRECTION ( 'NONE',  ( 0.000000000000000000, 0.000000000000000000, 1.000000000000000000 ) ) ;
#5271 = DIRECTION ( 'NONE',  ( 0.000000000000000000, 0.000000000000000000, 1.000000000000000000 ) ) ;
#5272 = ADVANCED_FACE ( 'NONE', ( #3430 ), #2645, .T. ) ;
#5273 = CARTESIAN_POINT ( 'NONE',  ( 35.00000000000000000, 90.00000000000000000, 1.000000000000003109 ) ) ;
#5274 = EDGE_CURVE ( 'NONE', #1701, #7344, #3371, .T. ) ;
#5275 = VERTEX_POINT ( 'NONE', #4605 ) ;
#5276 = PLANE ( 'NONE',  #11390 ) ;
#5277 = FACE_BOUND ( 'NONE', #5044, .T. ) ;
#5278 = ORIENTED_EDGE ( 'NONE', *, *, #11181, .T. ) ;
#5279 = AXIS2_PLACEMENT_3D ( 'NONE', #10792, #1832, #7847 ) ;
#5280 = DIRECTION ( 'NONE',  ( -0.3262398754384820965, 0.9452870165584017492, 0.000000000000000000 ) ) ;
#5281 = LINE ( 'NONE', #7179, #7024 ) ;
#5282 = VERTEX_POINT ( 'NONE', #3563 ) ;
#5283 = ORIENTED_EDGE ( 'NONE', *, *, #747, .F. ) ;
#5284 = DIRECTION ( 'NONE',  ( -1.000000000000000000, 0.000000000000000000, -5.337610695313252124E-17 ) ) ;
#5285 = DIRECTION ( 'NONE',  ( -1.000000000000000000, -0.000000000000000000, -0.000000000000000000 ) ) ;
#5286 = ORIENTED_EDGE ( 'NONE', *, *, #4123, .F. ) ;
#5287 = ADVANCED_BREP_SHAPE_REPRESENTATION ( '', ( #3386, #5704 ), #60 ) ;
#5288 = ORIENTED_EDGE ( 'NONE', *, *, #12761, .T. ) ;
#5289 = DIRECTION ( 'NONE',  ( 0.000000000000000000, 0.000000000000000000, 1.000000000000000000 ) ) ;
#5290 = PRODUCT_DEFINITION ( 'UNKNOWN', '', #1115, #9731 ) ;
#5291 = ORIENTED_EDGE ( 'NONE', *, *, #9934, .F. ) ;
#5292 = VECTOR ( 'NONE', #2933, 1000.000000000000000 ) ;
#5293 =( NAMED_UNIT ( * ) PLANE_ANGLE_UNIT ( ) SI_UNIT ( $, .RADIAN. ) );
#5294 = CARTESIAN_POINT ( 'NONE',  ( 60.63303222545420823, 111.5086687406912347, 2.829484441871016109 ) ) ;
#5295 = VERTEX_POINT ( 'NONE', #3500 ) ;
#5296 = ADVANCED_FACE ( 'NONE', ( #7543 ), #11230, .F. ) ;
#5297 = CARTESIAN_POINT ( 'NONE',  ( 1.040000000000000036, 0.5773502691896262862, -1.000000000000000000 ) ) ;
#5298 = ORIENTED_EDGE ( 'NONE', *, *, #5118, .T. ) ;
#5299 =( GEOMETRIC_REPRESENTATION_CONTEXT ( 3 ) GLOBAL_UNCERTAINTY_ASSIGNED_CONTEXT ( ( #4994 ) ) GLOBAL_UNIT_ASSIGNED_CONTEXT ( ( #3069, #8100, #12087 ) ) REPRESENTATION_CONTEXT ( 'NONE', 'WORKASPACE' ) );
#5300 = CARTESIAN_POINT ( 'NONE',  ( 9.999999999999994671, 27.00000000000000000, 2.500000000000000000 ) ) ;
#5301 = DIRECTION ( 'NONE',  ( 1.000000000000000000, 0.000000000000000000, 5.337610695313252124E-17 ) ) ;
#5302 = DIRECTION ( 'NONE',  ( 0.000000000000000000, 0.000000000000000000, 1.000000000000000000 ) ) ;
#5303 = CLOSED_SHELL ( 'NONE', ( #2353, #824, #3930, #12816, #1435, #12720, #7027, #8380, #3878, #4772, #11917, #3569, #2002, #4930, #3853, #1787, #1565, #6934, #11155, #12690, #10564, #6160, #125, #6870, #8492, #4484, #6867 ) ) ;
#5304 = CARTESIAN_POINT ( 'NONE',  ( -36.66666666666665009, 30.00000000000000000, -7.999999999999996447 ) ) ;
#5305 = ORIENTED_EDGE ( 'NONE', *, *, #8626, .T. ) ;
#5306 = DIRECTION ( 'NONE',  ( -1.000000000000000000, -0.000000000000000000, -0.000000000000000000 ) ) ;
#5307 = CARTESIAN_POINT ( 'NONE',  ( 19.40000000000002700, 62.98000740192551206, 4.625000000000000000 ) ) ;
#5308 = EDGE_CURVE ( 'NONE', #977, #11518, #9373, .T. ) ;
#5309 = CARTESIAN_POINT ( 'NONE',  ( 35.00000000000000000, 126.0266567974326222, 3.087499999999999911 ) ) ;
#5310 = ORIENTED_EDGE ( 'NONE', *, *, #3228, .T. ) ;
#5311 = VECTOR ( 'NONE', #12266, 1000.000000000000000 ) ;
#5312 = DIRECTION ( 'NONE',  ( -1.000000000000000000, 0.000000000000000000, 0.000000000000000000 ) ) ;
#5313 = PRODUCT ( 'motor', 'motor', '', ( #1169 ) ) ;
#5314 = EDGE_CURVE ( 'NONE', #7217, #3473, #7608, .T. ) ;
#5315 = VERTEX_POINT ( 'NONE', #461 ) ;
#5316 = LINE ( 'NONE', #12187, #2327 ) ;
#5317 = DIRECTION ( 'NONE',  ( -1.000000000000000000, 0.000000000000000000, 0.000000000000000000 ) ) ;
#5318 = CARTESIAN_POINT ( 'NONE',  ( -53.33333333333332149, 79.07477288111861924, 1.000000000000000888 ) ) ;
#5319 = LINE ( 'NONE', #4153, #3523 ) ;
#5320 = LINE ( 'NONE', #267, #4585 ) ;
#5321 = AXIS2_PLACEMENT_3D ( 'NONE', #3760, #8913, #11729 ) ;
#5322 = ADVANCED_FACE ( 'NONE', ( #2576 ), #6363, .T. ) ;
#5323 = LINE ( 'NONE', #11212, #6059 ) ;
#5324 = DIRECTION ( 'NONE',  ( -0.000000000000000000, -0.5000000000000003331, 0.8660254037844384856 ) ) ;
#5325 = CARTESIAN_POINT ( 'NONE',  ( -0.1038759689922479496, -3.348389132562988646, -0.8000000000000000444 ) ) ;
#5326 = DIRECTION ( 'NONE',  ( 0.5000000000000036637, -0.8660254037844365982, 0.000000000000000000 ) ) ;
#5327 = AXIS2_PLACEMENT_3D ( 'NONE', #7566, #5534, #554 ) ;
#5328 = CARTESIAN_POINT ( 'NONE',  ( 3.556430356250028790, 71.84604660189818048, 3.546875000614517326 ) ) ;
#5329 = EDGE_LOOP ( 'NONE', ( #8349, #9058, #5030 ) ) ;
#5330 = VECTOR ( 'NONE', #12492, 1000.000000000000000 ) ;
#5331 = LINE ( 'NONE', #2274, #10386 ) ;
#5332 = ORIENTED_EDGE ( 'NONE', *, *, #678, .F. ) ;
#5333 = LINE ( 'NONE', #7106, #5179 ) ;
#5334 = DIRECTION ( 'NONE',  ( 0.000000000000000000, 0.000000000000000000, 1.000000000000000000 ) ) ;
#5335 = VECTOR ( 'NONE', #4877, 1000.000000000000000 ) ;
#5336 = EDGE_CURVE ( 'NONE', #7167, #1692, #2050, .T. ) ;
#5337 = FACE_OUTER_BOUND ( 'NONE', #9194, .T. ) ;
#5338 = AXIS2_PLACEMENT_3D ( 'NONE', #8699, #1568, #11642 ) ;
#5339 = ORIENTED_EDGE ( 'NONE', *, *, #6683, .F. ) ;
#5340 = CARTESIAN_POINT ( 'NONE',  ( 6.499999999999999112, 70.70319397786906279, 0.9999999999999997780 ) ) ;
#5341 = DIRECTION ( 'NONE',  ( -0.000000000000000000, -0.000000000000000000, -1.000000000000000000 ) ) ;
#5342 = EDGE_LOOP ( 'NONE', ( #9076, #3347, #2462, #7249 ) ) ;
#5343 = CARTESIAN_POINT ( 'NONE',  ( 25.83484861008832567, 86.00000000000000000, -10.00000000000000000 ) ) ;
#5344 = ORIENTED_EDGE ( 'NONE', *, *, #10071, .T. ) ;
#5345 = ORIENTED_EDGE ( 'NONE', *, *, #11274, .F. ) ;
#5346 = ADVANCED_FACE ( 'NONE', ( #1657 ), #11400, .T. ) ;
#5347 = EDGE_CURVE ( 'NONE', #261, #7067, #8111, .T. ) ;
#5348 = MECHANICAL_DESIGN_GEOMETRIC_PRESENTATION_REPRESENTATION (  '', ( #10789 ), #10982 ) ;
#5349 = DIRECTION ( 'NONE',  ( -0.000000000000000000, 0.5000000000000000000, 0.8660254037844385966 ) ) ;
#5350 = CARTESIAN_POINT ( 'NONE',  ( 35.75000000000000711, 93.26496554346289258, -3.000000000000000000 ) ) ;
#5351 = ORIENTED_EDGE ( 'NONE', *, *, #5023, .T. ) ;
#5352 = VERTEX_POINT ( 'NONE', #4409 ) ;
#5353 = CARTESIAN_POINT ( 'NONE',  ( -23.49999999999999289, 79.07477288111861924, -1.000000000000000000 ) ) ;
#5354 = VERTEX_POINT ( 'NONE', #11463 ) ;
#5355 = DIRECTION ( 'NONE',  ( 0.000000000000000000, 0.000000000000000000, -1.000000000000000000 ) ) ;
#5356 = CARTESIAN_POINT ( 'NONE',  ( 19.40000000000000924, 117.0199925980744666, 4.137500001229033941 ) ) ;
#5357 = VECTOR ( 'NONE', #6489, 1000.000000000000000 ) ;
#5358 = ORIENTED_EDGE ( 'NONE', *, *, #4873, .F. ) ;
#5359 = CARTESIAN_POINT ( 'NONE',  ( 25.00000000000000355, 2.000000000000000000, 4.150000000000007461 ) ) ;
#5360 = EDGE_LOOP ( 'NONE', ( #312, #6700, #3303, #1844 ) ) ;
#5361 = CARTESIAN_POINT ( 'NONE',  ( 38.50000000000000711, 90.00000000000000000, -3.799999999999999378 ) ) ;
#5362 = ADVANCED_FACE ( 'NONE', ( #5645 ), #6148, .F. ) ;
#5363 = DIRECTION ( 'NONE',  ( 0.000000000000000000, 0.000000000000000000, -1.000000000000000000 ) ) ;
#5364 = SHAPE_REPRESENTATION_RELATIONSHIP ( 'NONE' , 'NONE' ,  #1066, #5287 ) ;
#5365 = VECTOR ( 'NONE', #11626, 1000.000000000000000 ) ;
#5366 = ADVANCED_FACE ( 'NONE', ( #5042 ), #9228, .T. ) ;
#5367 = ORIENTED_EDGE ( 'NONE', *, *, #10046, .T. ) ;
#5368 = CARTESIAN_POINT ( 'NONE',  ( 3.556430356250014579, 108.1539533981018053, 3.021875000614517415 ) ) ;
#5369 = ORIENTED_EDGE ( 'NONE', *, *, #1250, .T. ) ;
#5370 = CARTESIAN_POINT ( 'NONE',  ( 50.00000000000000000, 2.000000000000000000, 10.00000000000000000 ) ) ;
#5371 = CARTESIAN_POINT ( 'NONE',  ( 35.00000000000000711, 53.69209320379640360, 4.521875000614516971 ) ) ;
#5372 = VERTEX_POINT ( 'NONE', #11119 ) ;
#5373 = AXIS2_PLACEMENT_3D ( 'NONE', #10631, #4620, #8481 ) ;
#5374 = CARTESIAN_POINT ( 'NONE',  ( 7.500000000000000000, 30.00000000000000000, -1.499999999999999556 ) ) ;
#5375 = DIRECTION ( 'NONE',  ( 0.000000000000000000, 0.000000000000000000, -1.000000000000000000 ) ) ;
#5376 = DIRECTION ( 'NONE',  ( -0.000000000000000000, 0.4999999999999998890, -0.8660254037844387076 ) ) ;
#5377 = ADVANCED_FACE ( 'NONE', ( #53 ), #9160, .T. ) ;
#5378 = DIRECTION ( 'NONE',  ( 1.000000000000000000, 0.000000000000000000, 0.000000000000000000 ) ) ;
#5379 = CARTESIAN_POINT ( 'NONE',  ( 3.800000000000015365, 90.00000000000000000, 5.000000000000000000 ) ) ;
#5380 = CARTESIAN_POINT ( 'NONE',  ( 35.00000000000000000, 90.00000000000000000, 1.000000000000003553 ) ) ;
#5381 = EDGE_CURVE ( 'NONE', #7791, #6015, #10211, .T. ) ;
#5382 = CARTESIAN_POINT ( 'NONE',  ( 1.269999999999999796, -2.850000000000000533, -3.490243377569956061E-16 ) ) ;
#5383 = CARTESIAN_POINT ( 'NONE',  ( 21.49999999999998579, 90.00000000000000000, -10.00000000000000000 ) ) ;
#5384 = CYLINDRICAL_SURFACE ( 'NONE', #8033, 1.500000000000001332 ) ;
#5385 = CARTESIAN_POINT ( 'NONE',  ( 8.499999999999998224, 79.07477288111861924, 1.000000000000000000 ) ) ;
#5386 = LINE ( 'NONE', #405, #5647 ) ;
#5387 = CARTESIAN_POINT ( 'NONE',  ( -6.666666666666660745, 0.000000000000000000, 1.499999999999999556 ) ) ;
#5388 = VECTOR ( 'NONE', #6053, 1000.000000000000000 ) ;
#5389 = ORIENTED_EDGE ( 'NONE', *, *, #7780, .T. ) ;
#5390 = VECTOR ( 'NONE', #9682, 1000.000000000000000 ) ;
#5391 = DIRECTION ( 'NONE',  ( 1.000000000000000000, 0.000000000000000000, 5.337610695313252124E-17 ) ) ;
#5392 = EDGE_LOOP ( 'NONE', ( #12639, #10067, #12807, #3297 ) ) ;
#5393 = EDGE_CURVE ( 'NONE', #8351, #6459, #5172, .T. ) ;
#5394 = EDGE_CURVE ( 'NONE', #10844, #11492, #5807, .T. ) ;
#5395 = CARTESIAN_POINT ( 'NONE',  ( 40.00000000000000000, 121.2009999999999934, -1.499999999999999778 ) ) ;
#5396 = CARTESIAN_POINT ( 'NONE',  ( 7.266925300896119211, 98.48530999652632545, 4.000000000000000000 ) ) ;
#5397 = DIRECTION ( 'NONE',  ( 0.000000000000000000, 0.000000000000000000, 1.000000000000000000 ) ) ;
#5398 = CIRCLE ( 'NONE', #7076, 3.350000000000003642 ) ;
#5399 = ORIENTED_EDGE ( 'NONE', *, *, #3059, .F. ) ;
#5400 = DIRECTION ( 'NONE',  ( -5.624500927088228034E-17, 1.370729058197317775E-18, 1.000000000000000000 ) ) ;
#5401 = PLANE ( 'NONE',  #7101 ) ;
#5402 = ORIENTED_EDGE ( 'NONE', *, *, #8986, .F. ) ;
#5403 = DIRECTION ( 'NONE',  ( 1.000000000000000000, 0.000000000000000000, 0.000000000000000000 ) ) ;
#5404 = ORIENTED_EDGE ( 'NONE', *, *, #9909, .F. ) ;
#5405 = AXIS2_PLACEMENT_3D ( 'NONE', #2808, #3854, #7710 ) ;
#5406 = VERTEX_POINT ( 'NONE', #3094 ) ;
#5407 = ADVANCED_FACE ( 'NONE', ( #7073 ), #6149, .F. ) ;
#5408 = VECTOR ( 'NONE', #11600, 1000.000000000000000 ) ;
#5409 = DIRECTION ( 'NONE',  ( 0.000000000000000000, 0.000000000000000000, -1.000000000000000000 ) ) ;
#5410 = CARTESIAN_POINT ( 'NONE',  ( 20.00000000000000355, 0.000000000000000000, -10.00000000000000000 ) ) ;
#5411 = VERTEX_POINT ( 'NONE', #5241 ) ;
#5412 = PRODUCT_DEFINITION_CONTEXT ( 'detailed design', #3183, 'design' ) ;
#5413 = PRODUCT ( 'MAS-185', 'MAS-185', '', ( #12234 ) ) ;
#5414 = EDGE_LOOP ( 'NONE', ( #11866, #7784 ) ) ;
#5416 = FACE_OUTER_BOUND ( 'NONE', #6675, .T. ) ;
#5415 = VECTOR ( 'NONE', #12703, 1000.000000000000000 ) ;
#5417 = ORIENTED_EDGE ( 'NONE', *, *, #9418, .T. ) ;
#5418 = DIRECTION ( 'NONE',  ( -1.000000000000000000, 0.000000000000000000, -0.000000000000000000 ) ) ;
#5419 = ITEM_DEFINED_TRANSFORMATION ( 'NONE', 'NONE', #4472,  #5704 ) ;
#5420 = CARTESIAN_POINT ( 'NONE',  ( 3.800000000000015365, 108.0133283987163111, 2.825000001229034385 ) ) ;
#5421 = EDGE_LOOP ( 'NONE', ( #6119, #8184, #7466, #7187 ) ) ;
#5422 =( REPRESENTATION_RELATIONSHIP ('NONE','NONE', #1997, #9523 ) REPRESENTATION_RELATIONSHIP_WITH_TRANSFORMATION ( #832 )SHAPE_REPRESENTATION_RELATIONSHIP( ) );
#5423 = CARTESIAN_POINT ( 'NONE',  ( 35.00000000000000000, 90.00000000000000000, -3.000000000000000000 ) ) ;
#5424 = ORIENTED_EDGE ( 'NONE', *, *, #3846, .F. ) ;
#5425 = CARTESIAN_POINT ( 'NONE',  ( 1.000000000000000000, -4.873461295629625489, 0.000000000000000000 ) ) ;
#5426 = EDGE_LOOP ( 'NONE', ( #8513, #4502, #6856, #6611 ) ) ;
#5427 = FACE_OUTER_BOUND ( 'NONE', #7555, .T. ) ;
#5428 = VECTOR ( 'NONE', #4563, 1000.000000000000000 ) ;
#5429 = CARTESIAN_POINT ( 'NONE',  ( 35.00000000000000000, 90.00000000000000000, 4.800000000000000711 ) ) ;
#5430 = SURFACE_STYLE_USAGE ( .BOTH. , #11317 ) ;
#5431 = ORIENTED_EDGE ( 'NONE', *, *, #4811, .T. ) ;
#5432 = DIRECTION ( 'NONE',  ( 0.03100775193798453039, 0.9995191440486532741, -0.000000000000000000 ) ) ;
#5433 = ORIENTED_EDGE ( 'NONE', *, *, #2209, .T. ) ;
#5434 = EDGE_CURVE ( 'NONE', #252, #7199, #1180, .T. ) ;
#5435 = DIRECTION ( 'NONE',  ( -1.000000000000000000, 0.000000000000000000, 0.000000000000000000 ) ) ;
#5436 = EDGE_CURVE ( 'NONE', #9602, #2096, #1628, .T. ) ;
#5437 = VECTOR ( 'NONE', #6837, 1000.000000000000000 ) ;
#5438 = AXIS2_PLACEMENT_3D ( 'NONE', #8661, #1463, #7613 ) ;
#5439 = DIRECTION ( 'NONE',  ( 1.000000000000000000, 0.000000000000000000, -0.000000000000000000 ) ) ;
#5440 = ORIENTED_EDGE ( 'NONE', *, *, #2518, .F. ) ;
#5441 = DIRECTION ( 'NONE',  ( 1.000000000000000000, 0.000000000000000000, 0.000000000000000000 ) ) ;
#5442 = DIRECTION ( 'NONE',  ( -0.000000000000000000, -1.000000000000000000, -0.000000000000000000 ) ) ;
#5443 = CARTESIAN_POINT ( 'NONE',  ( 19.27821517812503060, 62.76906990284727783, 4.034375000614517148 ) ) ;
#5444 = DIRECTION ( 'NONE',  ( 0.000000000000000000, 0.000000000000000000, 1.000000000000000000 ) ) ;
#5445 = FACE_OUTER_BOUND ( 'NONE', #5555, .T. ) ;
#5446 = AXIS2_PLACEMENT_3D ( 'NONE', #394, #8397, #5184 ) ;
#5447 = CARTESIAN_POINT ( 'NONE',  ( 25.00000000000000355, -5.000000000000000000, -4.249999999999998224 ) ) ;
#5448 = CARTESIAN_POINT ( 'NONE',  ( 19.40000000000002700, 62.98000740192551206, 3.837500001229034563 ) ) ;
#5449 = DIRECTION ( 'NONE',  ( 0.000000000000000000, 0.000000000000000000, 1.000000000000000000 ) ) ;
#5450 = CARTESIAN_POINT ( 'NONE',  ( 1.040000000000000036, 0.000000000000000000, 0.000000000000000000 ) ) ;
#5451 = LINE ( 'NONE', #11607, #3885 ) ;
#5452 = VECTOR ( 'NONE', #2706, 1000.000000000000000 ) ;
#5453 = CARTESIAN_POINT ( 'NONE',  ( 31.86869970978804290, 88.80942934165229019, 4.000000000000000000 ) ) ;
#5454 = EDGE_CURVE ( 'NONE', #5809, #11221, #7593, .T. ) ;
#5455 = VERTEX_POINT ( 'NONE', #10344 ) ;
#5456 = DIRECTION ( 'NONE',  ( -1.000000000000000000, 0.000000000000000000, -0.000000000000000000 ) ) ;
#5457 = DIRECTION ( 'NONE',  ( 0.000000000000000000, 0.000000000000000000, 1.000000000000000000 ) ) ;
#5458 = EDGE_LOOP ( 'NONE', ( #171, #6907, #8383, #7426, #1378, #8238 ) ) ;
#5459 = CARTESIAN_POINT ( 'NONE',  ( 25.00000000000000355, 3.650000000000000355, -5.750000000000000000 ) ) ;
#5460 = DIRECTION ( 'NONE',  ( -1.000000000000000000, 0.000000000000000000, 0.000000000000000000 ) ) ;
#5461 = CARTESIAN_POINT ( 'NONE',  ( 19.40000000000002700, 62.98000740192551206, 4.625000000000000000 ) ) ;
#5462 = DIRECTION ( 'NONE',  ( 1.000000000000000000, 0.000000000000000000, 0.000000000000000000 ) ) ;
#5463 = VERTEX_POINT ( 'NONE', #1507 ) ;
#5464 = EDGE_CURVE ( 'NONE', #9108, #767, #10615, .T. ) ;
#5465 = DIRECTION ( 'NONE',  ( -0.000000000000000000, -1.000000000000000000, -0.000000000000000000 ) ) ;
#5466 = LINE ( 'NONE', #11422, #3144 ) ;
#5467 = ORIENTED_EDGE ( 'NONE', *, *, #4289, .F. ) ;
#5468 = PRESENTATION_STYLE_ASSIGNMENT (( #2476 ) ) ;
#5469 = DIRECTION ( 'NONE',  ( 0.000000000000000000, -0.000000000000000000, 1.000000000000000000 ) ) ;
#5470 = EDGE_CURVE ( 'NONE', #7589, #7127, #11581, .T. ) ;
#5471 = ORIENTED_EDGE ( 'NONE', *, *, #10260, .F. ) ;
#5472 = CIRCLE ( 'NONE', #12165, 1.599999999999999645 ) ;
#5473 = DIRECTION ( 'NONE',  ( 0.000000000000000000, 0.000000000000000000, 1.000000000000000000 ) ) ;
#5474 = ORIENTED_EDGE ( 'NONE', *, *, #10364, .T. ) ;
#5475 = LINE ( 'NONE', #2545, #7580 ) ;
#5476 = CARTESIAN_POINT ( 'NONE',  ( 5.000000000000004441, 30.00000000000000000, -10.00000000000000000 ) ) ;
#5477 = VERTEX_POINT ( 'NONE', #11316 ) ;
#5478 = PLANE ( 'NONE',  #270 ) ;
#5479 = VECTOR ( 'NONE', #2244, 1000.000000000000000 ) ;
#5480 = CYLINDRICAL_SURFACE ( 'NONE', #3880, 31.19999999999998863 ) ;
#5481 = EDGE_LOOP ( 'NONE', ( #4646, #3553, #5659, #1433 ) ) ;
#5482 = CARTESIAN_POINT ( 'NONE',  ( -15.06519709809452756, 92.38262548349219117, -0.9999999999999970024 ) ) ;
#5483 = APPLICATION_PROTOCOL_DEFINITION ( 'draft international standard', 'automotive_design', 1998, #904 ) ;
#5484 = CARTESIAN_POINT ( 'NONE',  ( 35.00000000000000711, 53.97334320256736362, 3.312500000000000000 ) ) ;
#5485 = EDGE_CURVE ( 'NONE', #4500, #7918, #6344, .T. ) ;
#5486 = ORIENTED_EDGE ( 'NONE', *, *, #5565, .T. ) ;
#5487 = LINE ( 'NONE', #10532, #2215 ) ;
#5488 = ORIENTED_EDGE ( 'NONE', *, *, #6703, .T. ) ;
#5489 = DIRECTION ( 'NONE',  ( 1.000000000000000000, 0.000000000000000000, 0.000000000000000000 ) ) ;
#5490 = ORIENTED_EDGE ( 'NONE', *, *, #5990, .F. ) ;
#5491 = CARTESIAN_POINT ( 'NONE',  ( 32.83880403052557284, 58.79641609890851583, 3.000000000000001776 ) ) ;
#5492 = MECHANICAL_DESIGN_GEOMETRIC_PRESENTATION_REPRESENTATION (  '', ( #4253 ), #5909 ) ;
#5493 = CARTESIAN_POINT ( 'NONE',  ( 34.25000000000000000, 92.49999999999998579, 6.000000000000000000 ) ) ;
#5494 = B_SPLINE_CURVE_WITH_KNOTS ( 'NONE', 3,
 ( #3007, #4965, #12226, #2092 ),
 .UNSPECIFIED., .F., .F.,
 ( 4, 4 ),
 ( 0.000000000000000000, 1.000000000000000000 ),
 .UNSPECIFIED. ) ;
#5495 = AXIS2_PLACEMENT_3D ( 'NONE', #11971, #7003, #46 ) ;
#5496 = ORIENTED_EDGE ( 'NONE', *, *, #5971, .F. ) ;
#5497 = CARTESIAN_POINT ( 'NONE',  ( 35.00000000000000000, 126.3079067962035822, 3.396875000614517415 ) ) ;
#5498 = ORIENTED_EDGE ( 'NONE', *, *, #9982, .T. ) ;
#5499 = CARTESIAN_POINT ( 'NONE',  ( 0.1038759689922479496, -3.348389132562988646, 0.000000000000000000 ) ) ;
#5500 = EDGE_CURVE ( 'NONE', #3649, #4047, #2630, .T. ) ;
#5501 = PRESENTATION_LAYER_ASSIGNMENT (  '', '', ( #12194 ) ) ;
#5502 = ORIENTED_EDGE ( 'NONE', *, *, #539, .T. ) ;
#5503 = SHAPE_REPRESENTATION ( 'base plate', ( #5704 ), #3631 ) ;
#5504 = CARTESIAN_POINT ( 'NONE',  ( 66.44356964374999563, 90.00000000000000000, 4.634375000614516793 ) ) ;
#5505 = ORIENTED_EDGE ( 'NONE', *, *, #12124, .F. ) ;
#5506 = LINE ( 'NONE', #3750, #1062 ) ;
#5507 = VECTOR ( 'NONE', #5866, 1000.000000000000000 ) ;
#5508 = DIRECTION ( 'NONE',  ( -0.8660254037844361541, -0.5000000000000042188, 0.000000000000000000 ) ) ;
#5509 = CARTESIAN_POINT ( 'NONE',  ( 35.00000000000000000, 126.3079067962036106, 2.946875000614516793 ) ) ;
#5510 = CARTESIAN_POINT ( 'NONE',  ( 3.556430356250015024, 90.00000000000000000, 4.353125000614517681 ) ) ;
#5511 = EDGE_CURVE ( 'NONE', #6093, #7515, #12574, .T. ) ;
#5512 = DIRECTION ( 'NONE',  ( 0.1305261922200528224, 0.9914448613738103822, 0.000000000000000000 ) ) ;
#5513 = ADVANCED_FACE ( 'NONE', ( #6605 ), #9488, .T. ) ;
#5514 = AXIS2_PLACEMENT_3D ( 'NONE', #12409, #489, #9337 ) ;
#5515 = DIRECTION ( 'NONE',  ( 0.8660254037844362651, 0.5000000000000042188, 0.000000000000000000 ) ) ;
#5516 = DIRECTION ( 'NONE',  ( -0.5000000000000044409, 0.8660254037844360431, 0.000000000000000000 ) ) ;
#5517 = CARTESIAN_POINT ( 'NONE',  ( -60.00000000000000000, 30.00000000000000000, -8.000000000000003553 ) ) ;
#5518 = DIRECTION ( 'NONE',  ( -0.000000000000000000, -0.000000000000000000, 1.000000000000000000 ) ) ;
#5519 = DIRECTION ( 'NONE',  ( -0.000000000000000000, 0.5000000000000003331, -0.8660254037844383745 ) ) ;
#5520 = LINE ( 'NONE', #4805, #4619 ) ;
#5521 = CARTESIAN_POINT ( 'NONE',  ( 35.00000000000000000, 90.00000000000000000, 6.000000000000000000 ) ) ;
#5522 = ORIENTED_EDGE ( 'NONE', *, *, #10037, .T. ) ;
#5523 = DIRECTION ( 'NONE',  ( 0.9995191440486532741, -0.03100775193798452692, 0.000000000000000000 ) ) ;
#5524 = DIRECTION ( 'NONE',  ( 0.000000000000000000, 0.000000000000000000, -1.000000000000000000 ) ) ;
#5525 = ORIENTED_EDGE ( 'NONE', *, *, #11663, .T. ) ;
#5526 = VECTOR ( 'NONE', #3823, 1000.000000000000000 ) ;
#5527 = PRODUCT_DEFINITION_SHAPE ( 'NONE', 'NONE',  #12955 ) ;
#5528 = VECTOR ( 'NONE', #12656, 1000.000000000000000 ) ;
#5529 = DIRECTION ( 'NONE',  ( 0.000000000000000000, 0.000000000000000000, 1.000000000000000000 ) ) ;
#5530 = CARTESIAN_POINT ( 'NONE',  ( 6.499999999999997335, 70.70319397786906279, -1.000000000000000888 ) ) ;
#5531 = ADVANCED_FACE ( 'NONE', ( #12305 ), #12370, .F. ) ;
#5532 = FACE_OUTER_BOUND ( 'NONE', #7173, .T. ) ;
#5533 = ORIENTED_EDGE ( 'NONE', *, *, #9064, .F. ) ;
#5534 = DIRECTION ( 'NONE',  ( -0.000000000000000000, 1.000000000000000000, -0.000000000000000000 ) ) ;
#5535 = LINE ( 'NONE', #4307, #12327 ) ;
#5536 = CIRCLE ( 'NONE', #10767, 3.500000000000003109 ) ;
#5537 = ORIENTED_EDGE ( 'NONE', *, *, #6307, .T. ) ;
#5538 = DIRECTION ( 'NONE',  ( 0.000000000000000000, 0.000000000000000000, 1.000000000000000000 ) ) ;
#5539 = FACE_OUTER_BOUND ( 'NONE', #1095, .T. ) ;
#5540 = ORIENTED_EDGE ( 'NONE', *, *, #7598, .T. ) ;
#5541 = DIRECTION ( 'NONE',  ( 0.8660254037844361541, 0.5000000000000042188, 0.000000000000000000 ) ) ;
#5542 = EDGE_LOOP ( 'NONE', ( #9539, #4617, #11160, #2305 ) ) ;
#5543 = DIRECTION ( 'NONE',  ( -1.000000000000000000, -0.000000000000000000, -0.000000000000000000 ) ) ;
#5544 = CARTESIAN_POINT ( 'NONE',  ( 1.040000000000000036, 0.000000000000000000, 0.000000000000000000 ) ) ;
#5545 = EDGE_LOOP ( 'NONE', ( #2093, #4389, #12867, #3999 ) ) ;
#5546 = VECTOR ( 'NONE', #11033, 1000.000000000000000 ) ;
#5547 = DIRECTION ( 'NONE',  ( 0.4719909656437444867, -0.8816033849473842166, 0.000000000000000000 ) ) ;
#5548 = EDGE_CURVE ( 'NONE', #1627, #1224, #1441, .T. ) ;
#5549 = VERTEX_POINT ( 'NONE', #9296 ) ;
#5550 = DIRECTION ( 'NONE',  ( -0.000000000000000000, 1.000000000000000000, -0.000000000000000000 ) ) ;
#5551 = ORIENTED_EDGE ( 'NONE', *, *, #12947, .F. ) ;
#5552 = FACE_OUTER_BOUND ( 'NONE', #11713, .T. ) ;
#5553 = SHAPE_DEFINITION_REPRESENTATION ( #7516, #5503 ) ;
#5554 = CARTESIAN_POINT ( 'NONE',  ( 19.40000000000000924, 117.0199925980744666, 3.687500001229034208 ) ) ;
#5555 = EDGE_LOOP ( 'NONE', ( #3274, #12408, #1448, #10203, #1381, #11819, #1222, #3673 ) ) ;
#5556 = AXIS2_PLACEMENT_3D ( 'NONE', #926, #10999, #6888 ) ;
#5557 = FILL_AREA_STYLE_COLOUR ( '', #8691 ) ;
#5558 = ORIENTED_EDGE ( 'NONE', *, *, #5856, .T. ) ;
#5559 = AXIS2_PLACEMENT_3D ( 'NONE', #6063, #2287, #7116 ) ;
#5560 = SURFACE_STYLE_USAGE ( .BOTH. , #7656 ) ;
#5561 = VERTEX_POINT ( 'NONE', #10409 ) ;
#5562 = CARTESIAN_POINT ( 'NONE',  ( 50.60000000000001563, 62.98000740192552627, 4.250000000000000000 ) ) ;
#5563 = CARTESIAN_POINT ( 'NONE',  ( 5.000000000000004441, 76.58915998087155685, -2.500000000000000000 ) ) ;
#5564 = EDGE_CURVE ( 'NONE', #3168, #2281, #319, .T. ) ;
#5565 = EDGE_CURVE ( 'NONE', #8709, #9125, #4525, .T. ) ;
#5566 = ORIENTED_EDGE ( 'NONE', *, *, #4067, .F. ) ;
#5567 = VECTOR ( 'NONE', #7235, 1000.000000000000114 ) ;
#5568 = CARTESIAN_POINT ( 'NONE',  ( 35.00000000000000000, 126.3079067962035822, 3.846875000614517592 ) ) ;
#5569 = ORIENTED_EDGE ( 'NONE', *, *, #3697, .F. ) ;
#5570 = CARTESIAN_POINT ( 'NONE',  ( 20.00000000000000355, 2.000000000000000000, -10.00000000000000000 ) ) ;
#5571 = EDGE_LOOP ( 'NONE', ( #5235, #10195, #9629, #2186 ) ) ;
#5572 = CARTESIAN_POINT ( 'NONE',  ( 66.44356964374999563, 71.84604660189820891, 3.696875000614517237 ) ) ;
#5573 = ORIENTED_EDGE ( 'NONE', *, *, #10170, .T. ) ;
#5574 = CARTESIAN_POINT ( 'NONE',  ( 35.00000000000000000, 90.00000000000000000, 4.000000000000000000 ) ) ;
#5575 = CARTESIAN_POINT ( 'NONE',  ( 7.321936442954655178, 105.0558282920940627, 3.000000000000000444 ) ) ;
#5576 = AXIS2_PLACEMENT_3D ( 'NONE', #2608, #8563, #4503 ) ;
#5577 = FILL_AREA_STYLE ('',( #6684 ) ) ;
#5578 = CARTESIAN_POINT ( 'NONE',  ( 40.00000000000000000, 2.000000000000001776, 1.500000000000001110 ) ) ;
#5579 = EDGE_CURVE ( 'NONE', #2666, #681, #2680, .T. ) ;
#5580 = DIRECTION ( 'NONE',  ( 0.000000000000000000, 0.000000000000000000, -1.000000000000000000 ) ) ;
#5581 = CARTESIAN_POINT ( 'NONE',  ( 50.00000000000000000, 2.000000000000000000, 10.00000000000000000 ) ) ;
#5582 = SHAPE_REPRESENTATION ( 'motor', ( #5704 ), #898 ) ;
#5583 = DIRECTION ( 'NONE',  ( -0.000000000000000000, -0.000000000000000000, -1.000000000000000000 ) ) ;
#5584 = DIRECTION ( 'NONE',  ( 0.000000000000000000, 0.000000000000000000, -1.000000000000000000 ) ) ;
#5585 = DIRECTION ( 'NONE',  ( 0.000000000000000000, 0.000000000000000000, 1.000000000000000000 ) ) ;
#5586 = VECTOR ( 'NONE', #5658, 1000.000000000000000 ) ;
#5587 = DIRECTION ( 'NONE',  ( -0.000000000000000000, -0.000000000000000000, -1.000000000000000000 ) ) ;
#5588 = ADVANCED_FACE ( 'NONE', ( #12506, #4588, #4394, #2500 ), #8582, .F. ) ;
#5589 = CARTESIAN_POINT ( 'NONE',  ( 66.19999999999998863, 90.00000000000000000, 3.425000000000000266 ) ) ;
#5590 = DIRECTION ( 'NONE',  ( 0.5000000000000038858, -0.8660254037844362651, 0.000000000000000000 ) ) ;
#5591 = ORIENTED_EDGE ( 'NONE', *, *, #6607, .F. ) ;
#5592 = CARTESIAN_POINT ( 'NONE',  ( 66.19999999999998863, 90.00000000000000000, 4.325000000000000178 ) ) ;
#5593 = LINE ( 'NONE', #8669, #11222 ) ;
#5594 = ORIENTED_EDGE ( 'NONE', *, *, #12195, .T. ) ;
#5595 = AXIS2_PLACEMENT_3D ( 'NONE', #10555, #7479, #6620 ) ;
#5596 = FILL_AREA_STYLE_COLOUR ( '', #8642 ) ;
#5597 = CARTESIAN_POINT ( 'NONE',  ( 3.556430356250015024, 90.00000000000000000, 4.831250000614517148 ) ) ;
#5598 =( REPRESENTATION_RELATIONSHIP ('NONE','NONE', #1997, #9523 ) REPRESENTATION_RELATIONSHIP_WITH_TRANSFORMATION ( #957 )SHAPE_REPRESENTATION_RELATIONSHIP( ) );
#5599 = CARTESIAN_POINT ( 'NONE',  ( 50.60000000000001563, 62.98000740192552627, 3.012500001229034829 ) ) ;
#5600 = ORIENTED_EDGE ( 'NONE', *, *, #9425, .T. ) ;
#5601 = FACE_OUTER_BOUND ( 'NONE', #5010, .T. ) ;
#5602 = ADVANCED_FACE ( 'NONE', ( #7397 ), #3484, .F. ) ;
#5603 = CARTESIAN_POINT ( 'NONE',  ( 5.000000000000005329, 67.52776749732610995, 2.500000000000000444 ) ) ;
#5604 = CIRCLE ( 'NONE', #4358, 30.19999999999999218 ) ;
#5605 = ADVANCED_FACE ( 'NONE', ( #6478 ), #3547, .F. ) ;
#5606 = ORIENTED_EDGE ( 'NONE', *, *, #622, .T. ) ;
#5607 = DIRECTION ( 'NONE',  ( 0.000000000000000000, 0.000000000000000000, -1.000000000000000000 ) ) ;
#5608 = CARTESIAN_POINT ( 'NONE',  ( -28.99038105676692112, 50.21281292110204930, -1.000000000000000000 ) ) ;
#5609 = VERTEX_POINT ( 'NONE', #2694 ) ;
#5610 = DIRECTION ( 'NONE',  ( 0.000000000000000000, -0.000000000000000000, -1.000000000000000000 ) ) ;
#5611 = ORIENTED_EDGE ( 'NONE', *, *, #1120, .F. ) ;
#5612 = DIRECTION ( 'NONE',  ( 0.000000000000000000, 0.000000000000000000, 1.000000000000000000 ) ) ;
#5613 = FACE_OUTER_BOUND ( 'NONE', #4181, .T. ) ;
#5614 = CIRCLE ( 'NONE', #4366, 1.000000000000000000 ) ;
#5615 = LINE ( 'NONE', #4639, #367 ) ;
#5616 = ORIENTED_EDGE ( 'NONE', *, *, #8358, .F. ) ;
#5617 = CARTESIAN_POINT ( 'NONE',  ( -38.66666666666665719, 2.000000000000000000, -7.999999999999996447 ) ) ;
#5618 = ORIENTED_EDGE ( 'NONE', *, *, #10898, .F. ) ;
#5619 = DIRECTION ( 'NONE',  ( 0.000000000000000000, 0.000000000000000000, -1.000000000000000000 ) ) ;
#5620 = APPLICATION_PROTOCOL_DEFINITION ( 'draft international standard', 'automotive_design', 1998, #2763 ) ;
#5621 = CARTESIAN_POINT ( 'NONE',  ( 19.40000000000000924, 117.0199925980744666, 3.237500001229034030 ) ) ;
#5622 = ORIENTED_EDGE ( 'NONE', *, *, #11633, .T. ) ;
#5623 = SURFACE_STYLE_USAGE ( .BOTH. , #8510 ) ;
#5624 = VERTEX_POINT ( 'NONE', #6799 ) ;
#5625 = VECTOR ( 'NONE', #1816, 1000.000000000000000 ) ;
#5626 = DIRECTION ( 'NONE',  ( -0.000000000000000000, -0.000000000000000000, -1.000000000000000000 ) ) ;
#5627 = ORIENTED_EDGE ( 'NONE', *, *, #8035, .T. ) ;
#5628 = EDGE_CURVE ( 'NONE', #1353, #9660, #785, .T. ) ;
#5629 = CARTESIAN_POINT ( 'NONE',  ( 44.79423261070191131, 60.36750792639232799, 3.000000000000000444 ) ) ;
#5630 = CARTESIAN_POINT ( 'NONE',  ( 0.000000000000000000, 0.000000000000000000, 1.499999999999998668 ) ) ;
#5631 = VECTOR ( 'NONE', #10799, 1000.000000000000000 ) ;
#5632 = AXIS2_PLACEMENT_3D ( 'NONE', #12838, #10867, #9887 ) ;
#5633 = ORIENTED_EDGE ( 'NONE', *, *, #4236, .F. ) ;
#5634 = CARTESIAN_POINT ( 'NONE',  ( 19.27821517812503060, 62.76906990284727783, 4.034375000614517148 ) ) ;
#5635 = EDGE_LOOP ( 'NONE', ( #9481, #10770 ) ) ;
#5636 = CARTESIAN_POINT ( 'NONE',  ( -60.00000000000000000, 30.00000000000000000, 7.999999999999996447 ) ) ;
#5637 = ORIENTED_EDGE ( 'NONE', *, *, #12153, .T. ) ;
#5638 = CARTESIAN_POINT ( 'NONE',  ( 3.556430356250014579, 108.1539533981018053, 4.821875000614516793 ) ) ;
#5639 = EDGE_LOOP ( 'NONE', ( #12167, #4141, #224 ) ) ;
#5640 = EDGE_CURVE ( 'NONE', #10525, #4968, #6995, .T. ) ;
#5641 = CARTESIAN_POINT ( 'NONE',  ( -3.666666666666661634, 79.07477288111861924, -1.000000000000000666 ) ) ;
#5642 = CARTESIAN_POINT ( 'NONE',  ( 64.31840976852106451, 100.6710284717588166, 2.999476386674974737 ) ) ;
#5643 = EDGE_CURVE ( 'NONE', #6259, #10216, #649, .T. ) ;
#5644 = LINE ( 'NONE', #4538, #10286 ) ;
#5645 = FACE_OUTER_BOUND ( 'NONE', #3855, .T. ) ;
#5646 = DIRECTION ( 'NONE',  ( 0.000000000000000000, 0.000000000000000000, -1.000000000000000000 ) ) ;
#5647 = VECTOR ( 'NONE', #5326, 1000.000000000000000 ) ;
#5648 = DIRECTION ( 'NONE',  ( 0.000000000000000000, 0.000000000000000000, 1.000000000000000000 ) ) ;
#5649 = CARTESIAN_POINT ( 'NONE',  ( 31.80092274341787828, 89.00581455129388075, 4.800000000000000711 ) ) ;
#5650 = PLANE ( 'NONE',  #1548 ) ;
#5651 = CARTESIAN_POINT ( 'NONE',  ( 35.75000000000000711, 93.26496554346289258, 4.800000000000000711 ) ) ;
#5652 = EDGE_CURVE ( 'NONE', #6677, #4357, #4145, .T. ) ;
#5653 = CARTESIAN_POINT ( 'NONE',  ( 3.556430356250015024, 90.00000000000000000, 4.803125000614516971 ) ) ;
#5654 = PLANE ( 'NONE',  #11416 ) ;
#5655 = ORIENTED_EDGE ( 'NONE', *, *, #5037, .F. ) ;
#5656 = CARTESIAN_POINT ( 'NONE',  ( 50.59999999999999432, 117.0199925980744666, 3.500000000000000444 ) ) ;
#5657 = AXIS2_PLACEMENT_3D ( 'NONE', #8978, #12125, #6890 ) ;
#5658 = DIRECTION ( 'NONE',  ( -0.4999999999999987232, 0.8660254037844393737, 0.000000000000000000 ) ) ;
#5659 = ORIENTED_EDGE ( 'NONE', *, *, #5394, .T. ) ;
#5660 =( BOUNDED_CURVE ( )  B_SPLINE_CURVE ( 2, ( #8622, #757, #6520, #8685, #2673, #10515, #12613 ),
 .UNSPECIFIED., .F., .F. ) 
 B_SPLINE_CURVE_WITH_KNOTS ( ( 3, 2, 2, 3 ),
 ( 0.1999999999999999833, 0.2333333333333333925, 0.2666666666666668295, 0.3000000000000002109 ),
 .UNSPECIFIED. ) 
 CURVE ( )  GEOMETRIC_REPRESENTATION_ITEM ( )  RATIONAL_B_SPLINE_CURVE ( ( 1.000000000000000222, 0.8660254037844385966, 1.000000000000000000, 0.8660254037844387076, 1.000000000000000000, 0.8660254037844378194, 1.000000000000000888 ) ) 
 REPRESENTATION_ITEM ( '' )  );
#5661 = CARTESIAN_POINT ( 'NONE',  ( 35.00000000000000000, 90.00000000000000000, 6.000000000000000000 ) ) ;
#5662 = CARTESIAN_POINT ( 'NONE',  ( 35.49999999999995026, 118.9978446673979704, 1.000000000000003109 ) ) ;
#5663 = COLOUR_RGB ( '',0.8941176470588234615, 0.8941176470588234615, 0.8941176470588234615 ) ;
#5664 = ORIENTED_EDGE ( 'NONE', *, *, #271, .T. ) ;
#5665 = DIRECTION ( 'NONE',  ( 0.000000000000000000, 0.000000000000000000, -1.000000000000000000 ) ) ;
#5666 = CARTESIAN_POINT ( 'NONE',  ( 3.556430356250014579, 108.1539533981018053, 4.315625000614517148 ) ) ;
#5667 = EDGE_CURVE ( 'NONE', #12821, #6093, #9811, .T. ) ;
#5668 = DIRECTION ( 'NONE',  ( -1.000000000000000000, -0.000000000000000000, 1.445602896647339348E-17 ) ) ;
#5669 = DIRECTION ( 'NONE',  ( 1.000000000000000000, 0.000000000000000000, 0.000000000000000000 ) ) ;
#5670 = ORIENTED_EDGE ( 'NONE', *, *, #3992, .T. ) ;
#5671 = CARTESIAN_POINT ( 'NONE',  ( 66.19999999999998863, 90.00000000000000000, 3.875000000000000000 ) ) ;
#5672 = ORIENTED_EDGE ( 'NONE', *, *, #6843, .T. ) ;
#5673 = CARTESIAN_POINT ( 'NONE',  ( 3.800000000000001155, 90.00000000000000000, -8.000000000000000000 ) ) ;
#5674 = AXIS2_PLACEMENT_3D ( 'NONE', #9522, #3139, #3447 ) ;
#5675 = CARTESIAN_POINT ( 'NONE',  ( 5.904717470405908664, 81.90651283295660789, 1.000000000000000000 ) ) ;
#5676 = B_SPLINE_CURVE_WITH_KNOTS ( 'NONE', 3,
 ( #11697, #5867, #4891, #2746 ),
 .UNSPECIFIED., .F., .F.,
 ( 4, 4 ),
 ( 0.000000000000000000, 1.000000000000000000 ),
 .UNSPECIFIED. ) ;
#5677 = EDGE_CURVE ( 'NONE', #1351, #1986, #4842, .T. ) ;
#5678 = EDGE_CURVE ( 'NONE', #7376, #2989, #10853, .T. ) ;
#5679 = PRODUCT_DEFINITION_CONTEXT ( 'detailed design', #904, 'design' ) ;
#5680 = LINE ( 'NONE', #8570, #580 ) ;
#5681 = ORIENTED_EDGE ( 'NONE', *, *, #8127, .F. ) ;
#5682 = CARTESIAN_POINT ( 'NONE',  ( 35.00000000000000000, 90.00000000000000000, 3.000000000000000000 ) ) ;
#5683 = ORIENTED_EDGE ( 'NONE', *, *, #5749, .F. ) ;
#5684 = CARTESIAN_POINT ( 'NONE',  ( 51.63999694657688622, 66.24635823768382181, 1.000000000000003109 ) ) ;
#5685 = APPLICATION_PROTOCOL_DEFINITION ( 'draft international standard', 'automotive_design', 1998, #8103 ) ;
#5686 = DIRECTION ( 'NONE',  ( 0.000000000000000000, 0.000000000000000000, 1.000000000000000000 ) ) ;
#5687 = ORIENTED_EDGE ( 'NONE', *, *, #11376, .F. ) ;
#5688 = PRESENTATION_LAYER_ASSIGNMENT (  '', '', ( #1930 ) ) ;
#5689 = DIRECTION ( 'NONE',  ( 0.000000000000000000, 0.8660254037844384856, -0.5000000000000004441 ) ) ;
#5690 = ORIENTED_EDGE ( 'NONE', *, *, #8588, .F. ) ;
#5691 = CARTESIAN_POINT ( 'NONE',  ( 0.000000000000000000, 0.4117131682837005258, -0.8000000000000000444 ) ) ;
#5692 = VERTEX_POINT ( 'NONE', #9869 ) ;
#5693 = CARTESIAN_POINT ( 'NONE',  ( 66.19999999999998863, 90.00000000000000000, 4.325000000000000178 ) ) ;
#5694 = LINE ( 'NONE', #840, #5390 ) ;
#5695 = VECTOR ( 'NONE', #6202, 1000.000000000000000 ) ;
#5696 = ORIENTED_EDGE ( 'NONE', *, *, #938, .T. ) ;
#5697 = CARTESIAN_POINT ( 'NONE',  ( 35.00000000000000000, 90.00000000000000000, 1.000000000000003109 ) ) ;
#5698 = ORIENTED_EDGE ( 'NONE', *, *, #2269, .F. ) ;
#5699 = EDGE_CURVE ( 'NONE', #10536, #7597, #5694, .T. ) ;
#5700 = CARTESIAN_POINT ( 'NONE',  ( 25.00000000000000355, 0.000000000000000000, -7.250000000000000888 ) ) ;
#5701 = ORIENTED_EDGE ( 'NONE', *, *, #11509, .T. ) ;
#5702 = CARTESIAN_POINT ( 'NONE',  ( 19.27821517812503060, 62.76906990284727783, 3.078125000614517326 ) ) ;
#5703 = ORIENTED_EDGE ( 'NONE', *, *, #7274, .T. ) ;
#5704 = AXIS2_PLACEMENT_3D ( 'NONE', #8997, #4824, #4886 ) ;
#5705 = LINE ( 'NONE', #1652, #8390 ) ;
#5706 = CARTESIAN_POINT ( 'NONE',  ( 5.000000000000004441, 30.00000000000000000, 2.500000000000000444 ) ) ;
#5707 = SURFACE_SIDE_STYLE ('',( #10680 ) ) ;
#5708 = CARTESIAN_POINT ( 'NONE',  ( 35.00000000000000711, 53.69209320379640360, 3.115625000614517415 ) ) ;
#5709 = EDGE_CURVE ( 'NONE', #7460, #8977, #4780, .T. ) ;
#5710 = CYLINDRICAL_SURFACE ( 'NONE', #2921, 31.19999999999998863 ) ;
#5711 = FACE_OUTER_BOUND ( 'NONE', #3140, .T. ) ;
#5712 = ADVANCED_FACE ( 'NONE', ( #11710 ), #12889, .T. ) ;
#5713 = CARTESIAN_POINT ( 'NONE',  ( -60.00000000000000000, 30.00000000000000000, -1.000000000000000000 ) ) ;
#5714 = CYLINDRICAL_SURFACE ( 'NONE', #5321, 3.350000000000000089 ) ;
#5715 = CIRCLE ( 'NONE', #1747, 31.19999999999999218 ) ;
#5716 = CARTESIAN_POINT ( 'NONE',  ( 35.00000000000000000, 90.00000000000000000, -1.000000000000000888 ) ) ;
#5717 = LINE ( 'NONE', #9580, #1478 ) ;
#5718 = CARTESIAN_POINT ( 'NONE',  ( 50.72178482187499071, 117.2309300971526937, 3.809375000614517504 ) ) ;
#5719 = ORIENTED_EDGE ( 'NONE', *, *, #12064, .T. ) ;
#5720 = CARTESIAN_POINT ( 'NONE',  ( 3.800000000000015365, 90.00000000000000000, 4.100000000000000533 ) ) ;
#5721 = CARTESIAN_POINT ( 'NONE',  ( 35.00000000000000000, 90.00000000000000000, -1.000000000000000000 ) ) ;
#5722 = ORIENTED_EDGE ( 'NONE', *, *, #2636, .T. ) ;
#5723 = VECTOR ( 'NONE', #2934, 1000.000000000000227 ) ;
#5724 = EDGE_CURVE ( 'NONE', #12575, #1209, #2947, .T. ) ;
#5725 = DIRECTION ( 'NONE',  ( -1.000000000000000000, 0.000000000000000000, 0.000000000000000000 ) ) ;
#5726 = DIRECTION ( 'NONE',  ( 0.000000000000000000, -1.000000000000000000, 0.000000000000000000 ) ) ;
#5727 = AXIS2_PLACEMENT_3D ( 'NONE', #2099, #3348, #11179 ) ;
#5728 = DIRECTION ( 'NONE',  ( 0.000000000000000000, 0.000000000000000000, 1.000000000000000000 ) ) ;
#5729 = DIRECTION ( 'NONE',  ( -0.000000000000000000, 1.000000000000000000, -0.000000000000000000 ) ) ;
#5730 = CARTESIAN_POINT ( 'NONE',  ( -57.55384757729342482, 35.76313972081443637, 1.836970198721030427E-16 ) ) ;
#5731 = LINE ( 'NONE', #2984, #8508 ) ;
#5732 = VERTEX_POINT ( 'NONE', #8826 ) ;
#5733 = LINE ( 'NONE', #6584, #549 ) ;
#5734 = ORIENTED_EDGE ( 'NONE', *, *, #7188, .T. ) ;
#5735 = CARTESIAN_POINT ( 'NONE',  ( 34.25000000000000000, 92.49999999999998579, -8.000000000000000000 ) ) ;
#5736 = DIRECTION ( 'NONE',  ( -1.000000000000000000, 0.000000000000000000, 0.000000000000000000 ) ) ;
#5737 = EDGE_CURVE ( 'NONE', #10107, #12599, #712, .T. ) ;
#5738 = DIRECTION ( 'NONE',  ( 0.03100775193798453039, 0.9995191440486532741, -0.000000000000000000 ) ) ;
#5739 = DIRECTION ( 'NONE',  ( 0.000000000000000000, 0.000000000000000000, -1.000000000000000000 ) ) ;
#5740 = AXIS2_PLACEMENT_3D ( 'NONE', #11891, #3132, #6853 ) ;
#5741 = LINE ( 'NONE', #3391, #1963 ) ;
#5742 = AXIS2_PLACEMENT_3D ( 'NONE', #12701, #11843, #3743 ) ;
#5743 = CARTESIAN_POINT ( 'NONE',  ( 35.00000000000000000, 90.00000000000000000, -1.000000000000000000 ) ) ;
#5744 = ORIENTED_EDGE ( 'NONE', *, *, #244, .F. ) ;
#5745 = CARTESIAN_POINT ( 'NONE',  ( 35.00000000000000000, 90.00000000000000000, 5.000000000000000000 ) ) ;
#5746 = CYLINDRICAL_SURFACE ( 'NONE', #11696, 10.00000000000000178 ) ;
#5747 = VERTEX_POINT ( 'NONE', #3740 ) ;
#5748 = PLANE ( 'NONE',  #6805 ) ;
#5749 = EDGE_CURVE ( 'NONE', #6072, #8571, #2758, .T. ) ;
#5750 = VERTEX_POINT ( 'NONE', #3933 ) ;
#5751 = EDGE_CURVE ( 'NONE', #3765, #488, #10603, .T. ) ;
#5752 = FILL_AREA_STYLE ('',( #11035 ) ) ;
#5754 = ORIENTED_EDGE ( 'NONE', *, *, #1016, .T. ) ;
#5753 = AXIS2_PLACEMENT_3D ( 'NONE', #6120, #10115, #7307 ) ;
#5755 = AXIS2_PLACEMENT_3D ( 'NONE', #6208, #239, #5092 ) ;
#5756 = DIRECTION ( 'NONE',  ( 5.624500927088228034E-17, -1.370729058197317775E-18, -1.000000000000000000 ) ) ;
#5757 = DIRECTION ( 'NONE',  ( -1.000000000000000000, -0.000000000000000000, -0.000000000000000000 ) ) ;
#5758 = ADVANCED_FACE ( 'NONE', ( #3803 ), #7782, .F. ) ;
#5759 = EDGE_LOOP ( 'NONE', ( #5017, #4127, #1648, #12677, #10198, #6739, #3425, #11611, #9417, #12912, #6780, #10968, #3621, #501, #3134, #492, #6263, #5389, #1452, #3939 ) ) ;
#5760 = CARTESIAN_POINT ( 'NONE',  ( 35.00000000000000000, 90.00000000000000000, 3.000000000000000000 ) ) ;
#5761 = ORIENTED_EDGE ( 'NONE', *, *, #5082, .T. ) ;
#5762 = VECTOR ( 'NONE', #7682, 1000.000000000000000 ) ;
#5763 = FACE_OUTER_BOUND ( 'NONE', #2688, .T. ) ;
#5764 = VECTOR ( 'NONE', #7563, 1000.000000000000000 ) ;
#5765 = ORIENTED_EDGE ( 'NONE', *, *, #2826, .T. ) ;
#5766 = FACE_BOUND ( 'NONE', #11360, .T. ) ;
#5767 = ORIENTED_EDGE ( 'NONE', *, *, #6976, .T. ) ;
#5768 = ADVANCED_FACE ( 'NONE', ( #1833 ), #899, .F. ) ;
#5769 = CARTESIAN_POINT ( 'NONE',  ( 19.40000000000000924, 117.0199925980744666, 4.025000000000000355 ) ) ;
#5770 = CARTESIAN_POINT ( 'NONE',  ( 25.00000000000000355, -5.000000000000000000, 5.750000000000000000 ) ) ;
#5771 = DIRECTION ( 'NONE',  ( 0.000000000000000000, 0.000000000000000000, 1.000000000000000000 ) ) ;
#5772 = CARTESIAN_POINT ( 'NONE',  ( 50.59999999999999432, 117.0199925980744666, 4.062500001229034652 ) ) ;
#5773 = AXIS2_PLACEMENT_3D ( 'NONE', #5080, #11491, #2413 ) ;
#5774 = PLANE ( 'NONE',  #11681 ) ;
#5775 = CARTESIAN_POINT ( 'NONE',  ( 6.000000000000008882, 90.00000000000000000, 4.000000000000000000 ) ) ;
#5776 = DIRECTION ( 'NONE',  ( 0.000000000000000000, -0.000000000000000000, 1.000000000000000000 ) ) ;
#5777 = DIRECTION ( 'NONE',  ( 0.000000000000000000, 0.000000000000000000, -1.000000000000000000 ) ) ;
#5778 = CARTESIAN_POINT ( 'NONE',  ( 1.040000000000000036, -0.5773502691896255090, 1.000000000000000000 ) ) ;
#5779 = LINE ( 'NONE', #6952, #5968 ) ;
#5780 = AXIS2_PLACEMENT_3D ( 'NONE', #7541, #5317, #11461 ) ;
#5781 = CARTESIAN_POINT ( 'NONE',  ( 35.75000000000000711, 93.41869858279433458, 4.800000000000000711 ) ) ;
#5782 = CARTESIAN_POINT ( 'NONE',  ( 3.556430356250015024, 90.00000000000000000, 3.509375000614517681 ) ) ;
#5783 = VERTEX_POINT ( 'NONE', #3077 ) ;
#5784 = CARTESIAN_POINT ( 'NONE',  ( 35.00000000000000711, 53.97334320256736362, 4.662499999999999645 ) ) ;
#5785 = CARTESIAN_POINT ( 'NONE',  ( 21.49999999999998579, 90.00000000000000000, -8.000000000000000000 ) ) ;
#5786 = ORIENTED_EDGE ( 'NONE', *, *, #9657, .T. ) ;
#5787 = ADVANCED_FACE ( 'NONE', ( #7056 ), #6004, .F. ) ;
#5788 = SHAPE_REPRESENTATION_RELATIONSHIP ( 'NONE' , 'NONE' ,  #11692, #2639 ) ;
#5789 = VECTOR ( 'NONE', #6682, 1000.000000000000000 ) ;
#5790 = FACE_OUTER_BOUND ( 'NONE', #8700, .T. ) ;
#5791 = FACE_BOUND ( 'NONE', #2355, .T. ) ;
#5792 = CYLINDRICAL_SURFACE ( 'NONE', #10971, 1.500000000000001332 ) ;
#5793 = CARTESIAN_POINT ( 'NONE',  ( 19.27821517812500574, 117.2309300971526937, 3.378125000614517148 ) ) ;
#5794 = DIRECTION ( 'NONE',  ( 0.8660254037844361541, 0.5000000000000042188, 0.000000000000000000 ) ) ;
#5795 = DIRECTION ( 'NONE',  ( 0.000000000000000000, 0.000000000000000000, -1.000000000000000000 ) ) ;
#5796 = EDGE_LOOP ( 'NONE', ( #2363, #8732, #3783, #2295, #11219 ) ) ;
#5797 = EDGE_CURVE ( 'NONE', #10652, #8374, #6130, .T. ) ;
#5798 = CIRCLE ( 'NONE', #8924, 1.500000000000001332 ) ;
#5799 = DIRECTION ( 'NONE',  ( 1.914177628664063178E-15, -1.000000000000000000, 0.000000000000000000 ) ) ;
#5800 = ORIENTED_EDGE ( 'NONE', *, *, #8822, .F. ) ;
#5801 = EDGE_CURVE ( 'NONE', #2940, #2177, #10124, .T. ) ;
#5802 = DIRECTION ( 'NONE',  ( -0.5000000000000044409, 0.8660254037844360431, 0.000000000000000000 ) ) ;
#5803 = CARTESIAN_POINT ( 'NONE',  ( 13.22666678878058200, 110.6378768499380527, -3.000000000000000000 ) ) ;
#5804 = DIRECTION ( 'NONE',  ( -0.000000000000000000, 1.000000000000000000, -0.000000000000000000 ) ) ;
#5805 = DIRECTION ( 'NONE',  ( 0.000000000000000000, 0.000000000000000000, 1.000000000000000000 ) ) ;
#5806 = FACE_OUTER_BOUND ( 'NONE', #11957, .T. ) ;
#5807 = CIRCLE ( 'NONE', #1416, 1.499999999999999556 ) ;
#5808 = CARTESIAN_POINT ( 'NONE',  ( -0.1698013801012111523, -5.473461295629626022, 0.000000000000000000 ) ) ;
#5809 = VERTEX_POINT ( 'NONE', #11039 ) ;
#5810 = LINE ( 'NONE', #27, #304 ) ;
#5811 = CARTESIAN_POINT ( 'NONE',  ( 28.50000000000000355, 90.00000000000000000, 4.000000000000000000 ) ) ;
#5812 = ORIENTED_EDGE ( 'NONE', *, *, #11735, .T. ) ;
#5813 = DIRECTION ( 'NONE',  ( 1.000000000000000000, 0.000000000000000000, 0.000000000000000000 ) ) ;
#5814 = ORIENTED_EDGE ( 'NONE', *, *, #1738, .F. ) ;
#5815 = ADVANCED_FACE ( 'NONE', ( #8108 ), #1094, .F. ) ;
#5816 = FACE_OUTER_BOUND ( 'NONE', #3455, .T. ) ;
#5817 = EDGE_LOOP ( 'NONE', ( #9553, #5690, #5283, #5600 ) ) ;
#5818 = VECTOR ( 'NONE', #12618, 1000.000000000000000 ) ;
#5819 = CARTESIAN_POINT ( 'NONE',  ( 0.000000000000000000, 1.836970198721029441E-16, -1.499999999999999556 ) ) ;
#5820 = CARTESIAN_POINT ( 'NONE',  ( 66.20000000000000284, 90.00000000000000000, 6.000000000000000000 ) ) ;
#5821 = EDGE_CURVE ( 'NONE', #3489, #587, #3950, .T. ) ;
#5822 = VERTEX_POINT ( 'NONE', #10975 ) ;
#5823 = CARTESIAN_POINT ( 'NONE',  ( 1.750000000000000000, 0.000000000000000000, 0.000000000000000000 ) ) ;
#5824 = ORIENTED_EDGE ( 'NONE', *, *, #9479, .T. ) ;
#5825 = DIRECTION ( 'NONE',  ( 1.000000000000000000, 0.000000000000000000, 0.000000000000000000 ) ) ;
#5826 = CONICAL_SURFACE ( 'NONE', #3117, 1.500000000000001332, 1.029744260000000411 ) ;
#5827 = VERTEX_POINT ( 'NONE', #5028 ) ;
#5828 = CARTESIAN_POINT ( 'NONE',  ( 66.44356964374999563, 71.84604660189820891, 4.540625000614517681 ) ) ;
#5829 = EDGE_LOOP ( 'NONE', ( #3976, #5345, #9432, #10892, #3865, #10472, #3875, #9237, #12490, #4576, #359, #4272, #9837, #12826, #10798, #3122, #6332, #227, #10800, #8411, #3342, #1619, #2338, #1716, #2439 ) ) ;
#5830 = LINE ( 'NONE', #6809, #1702 ) ;
#5831 = CARTESIAN_POINT ( 'NONE',  ( -36.66666666666665009, 2.000000000000000000, 7.999999999999998224 ) ) ;
#5832 = SURFACE_STYLE_USAGE ( .BOTH. , #4731 ) ;
#5833 = VECTOR ( 'NONE', #603, 999.9999999999998863 ) ;
#5834 = CARTESIAN_POINT ( 'NONE',  ( 3.800000000000015365, 108.0133283987163111, 4.625000001229034652 ) ) ;
#5835 = VECTOR ( 'NONE', #6748, 1000.000000000000000 ) ;
#5836 = DIRECTION ( 'NONE',  ( 0.03100775193798453039, -0.9995191440486532741, 0.000000000000000000 ) ) ;
#5837 = EDGE_CURVE ( 'NONE', #4915, #8617, #5604, .T. ) ;
#5839 = ADVANCED_FACE ( 'NONE', ( #4250 ), #5154, .T. ) ;
#5838 = DIRECTION ( 'NONE',  ( 1.000000000000000000, 0.000000000000000000, 0.000000000000000000 ) ) ;
#5840 = CARTESIAN_POINT ( 'NONE',  ( 31.59522469073172601, 84.46307801270442894, -0.9999999999999970024 ) ) ;
#5841 = DIRECTION ( 'NONE',  ( -0.3262398754384822630, 0.9452870165584014162, 0.000000000000000000 ) ) ;
#5842 = CARTESIAN_POINT ( 'NONE',  ( -48.33333333333332860, 0.000000000000000000, 1.499999999999999556 ) ) ;
#5843 = AXIS2_PLACEMENT_3D ( 'NONE', #8898, #5946, #6868 ) ;
#5844 = DIRECTION ( 'NONE',  ( 1.000000000000000000, 0.000000000000000000, 0.000000000000000000 ) ) ;
#5845 = ORIENTED_EDGE ( 'NONE', *, *, #349, .T. ) ;
#5846 = CARTESIAN_POINT ( 'NONE',  ( 36.50000000000001421, 67.79999999999999716, 6.000000000000000000 ) ) ;
#5847 = CARTESIAN_POINT ( 'NONE',  ( 50.72178482187499071, 117.2309300971526937, 4.259375000614517681 ) ) ;
#5848 = ORIENTED_EDGE ( 'NONE', *, *, #8018, .F. ) ;
#5849 = CARTESIAN_POINT ( 'NONE',  ( 62.73309762663101452, 98.48529854432332797, 1.000000000000003109 ) ) ;
#5850 = ORIENTED_EDGE ( 'NONE', *, *, #3565, .F. ) ;
#5851 = AXIS2_PLACEMENT_3D ( 'NONE', #7309, #487, #11489 ) ;
#5852 = FACE_OUTER_BOUND ( 'NONE', #5542, .T. ) ;
#5853 = PRODUCT_RELATED_PRODUCT_CATEGORY ( 'part', '', ( #4489 ) ) ;
#5854 = DIRECTION ( 'NONE',  ( 0.000000000000000000, -1.000000000000000000, 0.000000000000000000 ) ) ;
#5855 = CARTESIAN_POINT ( 'NONE',  ( 25.00000000000000355, 0.000000000000000000, -4.249999999999998224 ) ) ;
#5856 = EDGE_CURVE ( 'NONE', #11781, #7731, #5494, .T. ) ;
#5857 = CARTESIAN_POINT ( 'NONE',  ( 64.54728994471078352, 100.7543353520590870, 2.802601390178781404 ) ) ;
#5858 = CARTESIAN_POINT ( 'NONE',  ( 0.000000000000000000, 0.5773502691896263972, 1.000000000000000000 ) ) ;
#5859 = DIRECTION ( 'NONE',  ( -0.000000000000000000, -0.000000000000000000, -1.000000000000000000 ) ) ;
#5860 = VERTEX_POINT ( 'NONE', #9079 ) ;
#5861 = ORIENTED_EDGE ( 'NONE', *, *, #11783, .F. ) ;
#5862 = VECTOR ( 'NONE', #996, 1000.000000000000000 ) ;
#5863 = DIRECTION ( 'NONE',  ( -0.000000000000000000, -0.000000000000000000, -1.000000000000000000 ) ) ;
#5865 = EDGE_CURVE ( 'NONE', #3479, #4781, #7068, .T. ) ;
#5864 = DIRECTION ( 'NONE',  ( -0.000000000000000000, -0.000000000000000000, -1.000000000000000000 ) ) ;
#5866 = DIRECTION ( 'NONE',  ( -0.000000000000000000, -0.4999999999999999445, -0.8660254037844387076 ) ) ;
#5867 = CARTESIAN_POINT ( 'NONE',  ( 34.49999999999995026, 119.0000000000000000, 2.333333333333333481 ) ) ;
#5868 = ORIENTED_EDGE ( 'NONE', *, *, #3206, .T. ) ;
#5869 = LINE ( 'NONE', #5077, #11380 ) ;
#5870 = EDGE_CURVE ( 'NONE', #6375, #12765, #3113, .T. ) ;
#5871 = CONTEXT_DEPENDENT_SHAPE_REPRESENTATION ( #9686, #12015 ) ;
#5872 = DIRECTION ( 'NONE',  ( -0.000000000000000000, -0.000000000000000000, 1.000000000000000000 ) ) ;
#5873 = ORIENTED_EDGE ( 'NONE', *, *, #136, .T. ) ;
#5874 = LINE ( 'NONE', #5999, #3888 ) ;
#5875 = ORIENTED_EDGE ( 'NONE', *, *, #6796, .F. ) ;
#5876 = EDGE_LOOP ( 'NONE', ( #742, #7857, #6131, #1186 ) ) ;
#5877 = CARTESIAN_POINT ( 'NONE',  ( 65.00000000000000000, 117.5000000000001705, 1.000000000000003109 ) ) ;
#5878 = CARTESIAN_POINT ( 'NONE',  ( 34.25000000000000000, 92.49999999999998579, -9.802775637731997449 ) ) ;
#5879 = EDGE_CURVE ( 'NONE', #3526, #11890, #9015, .T. ) ;
#5880 = ORIENTED_EDGE ( 'NONE', *, *, #4458, .F. ) ;
#5881 = PRESENTATION_LAYER_ASSIGNMENT (  '', '', ( #11529 ) ) ;
#5882 = FACE_OUTER_BOUND ( 'NONE', #12700, .T. ) ;
#5883 = ORIENTED_EDGE ( 'NONE', *, *, #2815, .F. ) ;
#5884 = FACE_OUTER_BOUND ( 'NONE', #9945, .T. ) ;
#5885 = VERTEX_POINT ( 'NONE', #12161 ) ;
#5886 = CARTESIAN_POINT ( 'NONE',  ( 66.44356964374999563, 90.00000000000000000, 3.678125000614516971 ) ) ;
#5887 = ORIENTED_EDGE ( 'NONE', *, *, #1625, .F. ) ;
#5888 = DIRECTION ( 'NONE',  ( -1.000000000000000000, -0.000000000000000000, -0.000000000000000000 ) ) ;
#5889 = CARTESIAN_POINT ( 'NONE',  ( 48.49999999999995737, 90.00000000000000000, -8.000000000000000000 ) ) ;
#5890 = CARTESIAN_POINT ( 'NONE',  ( 3.800000000000015365, 90.00000000000000000, 3.312500001229034652 ) ) ;
#5891 = MECHANICAL_DESIGN_GEOMETRIC_PRESENTATION_REPRESENTATION (  '', ( #8407 ), #5051 ) ;
#5892 = CARTESIAN_POINT ( 'NONE',  ( 50.59999999999999432, 117.0199925980744666, 4.512500001229033941 ) ) ;
#5893 = CARTESIAN_POINT ( 'NONE',  ( 5.904717470405909552, 81.90651283295660789, -1.000000000000000000 ) ) ;
#5894 = ADVANCED_FACE ( 'NONE', ( #7978 ), #167, .F. ) ;
#5895 = ORIENTED_EDGE ( 'NONE', *, *, #5865, .T. ) ;
#5896 = CARTESIAN_POINT ( 'NONE',  ( 35.75000000000000711, 92.49999999999998579, 4.000000000000000000 ) ) ;
#5897 = DIRECTION ( 'NONE',  ( 0.000000000000000000, 0.000000000000000000, 1.000000000000000000 ) ) ;
#5898 = CARTESIAN_POINT ( 'NONE',  ( 35.00000000000000000, 90.00000000000000000, 1.000000000000003553 ) ) ;
#5899 = ORIENTED_EDGE ( 'NONE', *, *, #11930, .F. ) ;
#5900 = VECTOR ( 'NONE', #12556, 1000.000000000000000 ) ;
#5901 = PLANE ( 'NONE',  #8644 ) ;
#5902 = ORIENTED_EDGE ( 'NONE', *, *, #6427, .F. ) ;
#5903 = DIRECTION ( 'NONE',  ( 0.5000000000000036637, -0.8660254037844365982, 0.000000000000000000 ) ) ;
#5905 = EDGE_CURVE ( 'NONE', #10261, #8824, #6071, .T. ) ;
#5904 = VERTEX_POINT ( 'NONE', #10193 ) ;
#5906 = ADVANCED_FACE ( 'NONE', ( #12950 ), #6989, .F. ) ;
#5907 = CARTESIAN_POINT ( 'NONE',  ( 66.44356964374998142, 108.1539533981018053, 4.221875000614517148 ) ) ;
#5908 = CARTESIAN_POINT ( 'NONE',  ( -56.05384757729341061, 33.16506350946112036, 0.000000000000000000 ) ) ;
#5909 =( GEOMETRIC_REPRESENTATION_CONTEXT ( 3 ) GLOBAL_UNCERTAINTY_ASSIGNED_CONTEXT ( ( #3485 ) ) GLOBAL_UNIT_ASSIGNED_CONTEXT ( ( #761, #3847, #6844 ) ) REPRESENTATION_CONTEXT ( 'NONE', 'WORKASPACE' ) );
#5910 = LINE ( 'NONE', #1003, #1551 ) ;
#5911 = EDGE_CURVE ( 'NONE', #7597, #12207, #7278, .T. ) ;
#5912 = FACE_OUTER_BOUND ( 'NONE', #5918, .T. ) ;
#5913 = LINE ( 'NONE', #3775, #6177 ) ;
#5914 = CARTESIAN_POINT ( 'NONE',  ( 63.99885733073619321, 89.74256357754357794, 1.000000000000003109 ) ) ;
#5915 = LINE ( 'NONE', #3780, #1600 ) ;
#5916 = VERTEX_POINT ( 'NONE', #10324 ) ;
#5917 = DIRECTION ( 'NONE',  ( 0.000000000000000000, 0.000000000000000000, -1.000000000000000000 ) ) ;
#5918 = EDGE_LOOP ( 'NONE', ( #3120, #12904, #592, #5734 ) ) ;
#5919 = VECTOR ( 'NONE', #4303, 1000.000000000000000 ) ;
#5920 = CARTESIAN_POINT ( 'NONE',  ( 38.50000000000000000, 90.00000000000000000, 4.000000000000000000 ) ) ;
#5921 = EDGE_CURVE ( 'NONE', #309, #6649, #1639, .T. ) ;
#5922 = MECHANICAL_DESIGN_GEOMETRIC_PRESENTATION_REPRESENTATION (  '', ( #8444 ), #4063 ) ;
#5923 = DIRECTION ( 'NONE',  ( 0.000000000000000000, -1.000000000000000000, 0.000000000000000000 ) ) ;
#5924 = CARTESIAN_POINT ( 'NONE',  ( -3.666666666666651420, 64.83346624110779999, 2.999999999999900968 ) ) ;
#5925 = DIRECTION ( 'NONE',  ( 0.000000000000000000, -1.000000000000000000, 0.000000000000000000 ) ) ;
#5926 = EDGE_LOOP ( 'NONE', ( #6440, #5351, #10447, #4430, #1630, #1955, #12233, #6487, #12489, #6126 ) ) ;
#5927 = CIRCLE ( 'NONE', #10108, 1.500000000000001332 ) ;
#5928 = LINE ( 'NONE', #10842, #10757 ) ;
#5929 = DIRECTION ( 'NONE',  ( 1.000000000000000000, 0.000000000000000000, 0.000000000000000000 ) ) ;
#5930 = AXIS2_PLACEMENT_3D ( 'NONE', #5597, #550, #11484 ) ;
#5931 = ORIENTED_EDGE ( 'NONE', *, *, #11969, .F. ) ;
#5932 =( NAMED_UNIT ( * ) PLANE_ANGLE_UNIT ( ) SI_UNIT ( $, .RADIAN. ) );
#5933 = SURFACE_STYLE_USAGE ( .BOTH. , #4774 ) ;
#5934 = ORIENTED_EDGE ( 'NONE', *, *, #11340, .T. ) ;
#5935 = CARTESIAN_POINT ( 'NONE',  ( 19.40000000000002700, 62.98000740192551206, 2.937500001229034208 ) ) ;
#5936 = CARTESIAN_POINT ( 'NONE',  ( 35.00000000000000000, 90.00000000000000000, 6.000000000000000000 ) ) ;
#5937 = VERTEX_POINT ( 'NONE', #5350 ) ;
#5938 = DIRECTION ( 'NONE',  ( 1.000000000000000000, 0.000000000000000000, 0.000000000000000000 ) ) ;
#5939 = CARTESIAN_POINT ( 'NONE',  ( 25.00000000000000355, 0.000000000000000000, 5.750000000000000000 ) ) ;
#5940 = ADVANCED_FACE ( 'NONE', ( #565 ), #7316, .T. ) ;
#5941 = VERTEX_POINT ( 'NONE', #5410 ) ;
#5942 = AXIS2_PLACEMENT_3D ( 'NONE', #5697, #7851, #1899 ) ;
#5943 = ORIENTED_EDGE ( 'NONE', *, *, #2283, .F. ) ;
#5944 = CARTESIAN_POINT ( 'NONE',  ( 0.000000000000000000, 0.5773502691896263972, 1.000000000000000000 ) ) ;
#5945 = ORIENTED_EDGE ( 'NONE', *, *, #8210, .T. ) ;
#5946 = DIRECTION ( 'NONE',  ( -0.000000000000000000, -0.000000000000000000, -1.000000000000000000 ) ) ;
#5947 = ORIENTED_EDGE ( 'NONE', *, *, #8951, .T. ) ;
#5948 = VECTOR ( 'NONE', #2730, 1000.000000000000000 ) ;
#5949 = CARTESIAN_POINT ( 'NONE',  ( 3.556430356250014579, 108.1539533981018053, 4.765625000614517326 ) ) ;
#5950 = ORIENTED_EDGE ( 'NONE', *, *, #5579, .T. ) ;
#5951 = AXIS2_PLACEMENT_3D ( 'NONE', #2158, #12837, #3998 ) ;
#5952 = CARTESIAN_POINT ( 'NONE',  ( 4.336808689942017736E-16, 1.424999999999999600, 0.000000000000000000 ) ) ;
#5953 = LINE ( 'NONE', #9950, #9551 ) ;
#5954 = EDGE_CURVE ( 'NONE', #9993, #2096, #6393, .T. ) ;
#5955 = CARTESIAN_POINT ( 'NONE',  ( 50.72178482187501203, 62.76906990284730625, 4.053125000614517859 ) ) ;
#5956 = EDGE_CURVE ( 'NONE', #5149, #6664, #792, .T. ) ;
#5957 = AXIS2_PLACEMENT_3D ( 'NONE', #4031, #2792, #7818 ) ;
#5958 = CARTESIAN_POINT ( 'NONE',  ( 6.000000000000008882, 90.00000000000000000, -1.000000000000000000 ) ) ;
#5959 = EDGE_LOOP ( 'NONE', ( #689, #520 ) ) ;
#5960 = VECTOR ( 'NONE', #11485, 1000.000000000000000 ) ;
#5961 = DIRECTION ( 'NONE',  ( -0.000000000000000000, -0.000000000000000000, -1.000000000000000000 ) ) ;
#5962 = DIRECTION ( 'NONE',  ( -0.000000000000000000, -0.000000000000000000, 1.000000000000000000 ) ) ;
#5963 = CARTESIAN_POINT ( 'NONE',  ( 18.66882170374126915, 116.8715781131384688, 3.000000000000000000 ) ) ;
#5964 = ORIENTED_EDGE ( 'NONE', *, *, #5454, .F. ) ;
#5965 = DIRECTION ( 'NONE',  ( 1.000000000000000000, 0.000000000000000000, 0.000000000000000000 ) ) ;
#5966 = ORIENTED_EDGE ( 'NONE', *, *, #8244, .F. ) ;
#5967 = FACE_OUTER_BOUND ( 'NONE', #7059, .T. ) ;
#5968 = VECTOR ( 'NONE', #11730, 1000.000000000000000 ) ;
#5969 = CARTESIAN_POINT ( 'NONE',  ( 50.72178482187501203, 62.76906990284730625, 4.109375000614517326 ) ) ;
#5970 = ORIENTED_EDGE ( 'NONE', *, *, #3165, .F. ) ;
#5971 = EDGE_CURVE ( 'NONE', #7840, #4911, #6328, .T. ) ;
#5972 = AXIS2_PLACEMENT_3D ( 'NONE', #2346, #1223, #9205 ) ;
#5973 = CARTESIAN_POINT ( 'NONE',  ( 19.27821517812503060, 62.76906990284727783, 3.134375000614517237 ) ) ;
#5974 = CARTESIAN_POINT ( 'NONE',  ( 19.40000000000000924, 117.0199925980744666, 3.687500001229034208 ) ) ;
#5975 = EDGE_CURVE ( 'NONE', #10262, #2828, #366, .T. ) ;
#5976 = DIRECTION ( 'NONE',  ( 0.000000000000000000, 0.000000000000000000, 1.000000000000000000 ) ) ;
#5977 = DIRECTION ( 'NONE',  ( 0.000000000000000000, -0.000000000000000000, -1.000000000000000000 ) ) ;
#5978 = EDGE_CURVE ( 'NONE', #9167, #4104, #1002, .T. ) ;
#5979 = VECTOR ( 'NONE', #1667, 1000.000000000000000 ) ;
#5980 = DIRECTION ( 'NONE',  ( 0.000000000000000000, 0.000000000000000000, 1.000000000000000000 ) ) ;
#5981 = CARTESIAN_POINT ( 'NONE',  ( 35.00000000000000000, 90.00000000000000000, -18.00000000000000355 ) ) ;
#5982 = FACE_OUTER_BOUND ( 'NONE', #8587, .T. ) ;
#5983 = ORIENTED_EDGE ( 'NONE', *, *, #8684, .T. ) ;
#5984 = FACE_OUTER_BOUND ( 'NONE', #11487, .T. ) ;
#5985 = ORIENTED_EDGE ( 'NONE', *, *, #8530, .T. ) ;
#5986 = AXIS2_PLACEMENT_3D ( 'NONE', #7038, #8023, #6050 ) ;
#5987 = DIRECTION ( 'NONE',  ( -5.624500927088228034E-17, 1.370729058197317775E-18, 1.000000000000000000 ) ) ;
#5988 = LINE ( 'NONE', #4827, #9365 ) ;
#5989 = CARTESIAN_POINT ( 'NONE',  ( -60.00000000000000000, 30.00000000000000000, 2.500000000000000000 ) ) ;
#5990 = EDGE_CURVE ( 'NONE', #10917, #2123, #3278, .T. ) ;
#5991 = DIRECTION ( 'NONE',  ( 0.000000000000000000, -0.000000000000000000, 1.000000000000000000 ) ) ;
#5992 = ADVANCED_FACE ( 'NONE', ( #3468 ), #2292, .T. ) ;
#5993 = VERTEX_POINT ( 'NONE', #3400 ) ;
#5994 = LINE ( 'NONE', #1948, #8677 ) ;
#5995 = LINE ( 'NONE', #2218, #4393 ) ;
#5996 = VECTOR ( 'NONE', #8011, 1000.000000000000000 ) ;
#5997 = ORIENTED_EDGE ( 'NONE', *, *, #5485, .F. ) ;
#5998 = SHAPE_REPRESENTATION_RELATIONSHIP ( 'NONE' , 'NONE' ,  #9014, #12938 ) ;
#5999 = CARTESIAN_POINT ( 'NONE',  ( -62.42520044359213927, 28.59980987105325667, -0.9999999999999928946 ) ) ;
#6000 = ORIENTED_EDGE ( 'NONE', *, *, #5223, .T. ) ;
#6001 = CARTESIAN_POINT ( 'NONE',  ( 6.500000000000000000, 68.39379290111055809, -1.000000000000000222 ) ) ;
#6002 = ORIENTED_EDGE ( 'NONE', *, *, #7724, .F. ) ;
#6003 = CARTESIAN_POINT ( 'NONE',  ( 19.40000000000002700, 62.98000740192551206, 4.174999999999999822 ) ) ;
#6004 = PLANE ( 'NONE',  #9584 ) ;
#6005 = ORIENTED_EDGE ( 'NONE', *, *, #4184, .F. ) ;
#6006 = AXIS2_PLACEMENT_3D ( 'NONE', #7532, #11385, #10538 ) ;
#6007 = EDGE_LOOP ( 'NONE', ( #1026, #10465, #2428, #11084 ) ) ;
#6008 = DIRECTION ( 'NONE',  ( 0.000000000000000000, 0.000000000000000000, -1.000000000000000000 ) ) ;
#6009 = ORIENTED_EDGE ( 'NONE', *, *, #10530, .F. ) ;
#6010 = CARTESIAN_POINT ( 'NONE',  ( 3.556430356250015024, 90.00000000000000000, 4.353125000614517681 ) ) ;
#6011 = EDGE_LOOP ( 'NONE', ( #4711, #969, #10869, #3187 ) ) ;
#6012 = DIRECTION ( 'NONE',  ( 0.000000000000000000, 0.000000000000000000, 1.000000000000000000 ) ) ;
#6013 = ADVANCED_FACE ( 'NONE', ( #10456 ), #8431, .T. ) ;
#6014 = CIRCLE ( 'NONE', #4562, 29.99999999999999645 ) ;
#6015 = VERTEX_POINT ( 'NONE', #10391 ) ;
#6016 = VECTOR ( 'NONE', #5285, 1000.000000000000000 ) ;
#6017 = CARTESIAN_POINT ( 'NONE',  ( -60.00000000000000000, 30.00000000000000000, 9.999999999999996447 ) ) ;
#6018 = CARTESIAN_POINT ( 'NONE',  ( 3.556430356250028790, 71.84604660189818048, 4.390625000614517326 ) ) ;
#6019 = CARTESIAN_POINT ( 'NONE',  ( 35.00000000000000000, 126.0266567974326222, 4.887499999999999289 ) ) ;
#6020 = DIRECTION ( 'NONE',  ( 0.000000000000000000, 0.000000000000000000, 1.000000000000000000 ) ) ;
#6021 = CARTESIAN_POINT ( 'NONE',  ( -60.00000000000000000, 30.00000000000000000, -3.000000000000000000 ) ) ;
#6022 = VECTOR ( 'NONE', #12263, 1000.000000000000000 ) ;
#6023 = ORIENTED_EDGE ( 'NONE', *, *, #11632, .T. ) ;
#6024 = CARTESIAN_POINT ( 'NONE',  ( 3.800000000000015365, 90.00000000000000000, 3.200000000000000178 ) ) ;
#6025 = EDGE_CURVE ( 'NONE', #4270, #5411, #4315, .T. ) ;
#6026 = EDGE_CURVE ( 'NONE', #261, #9467, #6267, .T. ) ;
#6027 = DIRECTION ( 'NONE',  ( -1.000000000000000000, 0.000000000000000000, 0.000000000000000000 ) ) ;
#6028 = CARTESIAN_POINT ( 'NONE',  ( 55.18046915913835448, 113.8894995096903955, 3.000000000000000888 ) ) ;
#6029 = EDGE_LOOP ( 'NONE', ( #4927, #12169, #6569, #7909 ) ) ;
#6030 = CARTESIAN_POINT ( 'NONE',  ( 28.99095782554746847, 92.47818727009294548, 22.38477631085024555 ) ) ;
#6031 = EDGE_CURVE ( 'NONE', #8114, #4915, #1422, .T. ) ;
#6032 = ORIENTED_EDGE ( 'NONE', *, *, #422, .F. ) ;
#6033 = VECTOR ( 'NONE', #7801, 1000.000000000000000 ) ;
#6034 = CARTESIAN_POINT ( 'NONE',  ( 35.49999999999995026, 119.0000000000000000, 4.000000000000000000 ) ) ;
#6035 = CARTESIAN_POINT ( 'NONE',  ( 50.72178482187499071, 117.2309300971526937, 3.303125000614517415 ) ) ;
#6036 = ORIENTED_EDGE ( 'NONE', *, *, #149, .T. ) ;
#6037 = VECTOR ( 'NONE', #7389, 1000.000000000000000 ) ;
#6038 = CARTESIAN_POINT ( 'NONE',  ( 3.556430356250028790, 71.84604660189818048, 3.996875000614517059 ) ) ;
#6039 = CYLINDRICAL_SURFACE ( 'NONE', #10196, 1.599999999999993872 ) ;
#6040 = LINE ( 'NONE', #10033, #156 ) ;
#6041 = VECTOR ( 'NONE', #10477, 1000.000000000000000 ) ;
#6042 = CYLINDRICAL_SURFACE ( 'NONE', #1758, 1.599999999999992095 ) ;
#6043 = EDGE_CURVE ( 'NONE', #9467, #10383, #9405, .T. ) ;
#6044 = DIRECTION ( 'NONE',  ( 0.000000000000000000, 0.000000000000000000, -1.000000000000000000 ) ) ;
#6045 = CARTESIAN_POINT ( 'NONE',  ( 45.00000000000000000, 0.000000000000000000, 5.750000000000000888 ) ) ;
#6046 = LINE ( 'NONE', #2005, #10663 ) ;
#6047 = PLANE ( 'NONE',  #4537 ) ;
#6048 = ORIENTED_EDGE ( 'NONE', *, *, #8793, .T. ) ;
#6049 = AXIS2_PLACEMENT_3D ( 'NONE', #12809, #7839, #5929 ) ;
#6050 = DIRECTION ( 'NONE',  ( 0.5000000000000038858, -0.8660254037844362651, 0.000000000000000000 ) ) ;
#6051 = ORIENTED_EDGE ( 'NONE', *, *, #1799, .T. ) ;
#6052 = SURFACE_STYLE_USAGE ( .BOTH. , #947 ) ;
#6053 = DIRECTION ( 'NONE',  ( -0.000000000000000000, -0.000000000000000000, -1.000000000000000000 ) ) ;
#6054 = DIRECTION ( 'NONE',  ( -0.8660254037844361541, -0.5000000000000042188, 9.389466242107213130E-17 ) ) ;
#6055 = ADVANCED_FACE ( 'NONE', ( #7449 ), #11431, .T. ) ;
#6056 = CARTESIAN_POINT ( 'NONE',  ( 18.35873618070580093, 66.24461453698026503, 4.000000000000000000 ) ) ;
#6057 = CIRCLE ( 'NONE', #9054, 4.000000000000003553 ) ;
#6058 = ORIENTED_EDGE ( 'NONE', *, *, #6326, .F. ) ;
#6059 = VECTOR ( 'NONE', #8341, 1000.000000000000000 ) ;
#6060 = CARTESIAN_POINT ( 'NONE',  ( 45.00000000000000000, 2.000000000000001332, 5.750000000000000888 ) ) ;
#6061 = DIRECTION ( 'NONE',  ( -0.000000000000000000, -0.000000000000000000, -1.000000000000000000 ) ) ;
#6062 = VERTEX_POINT ( 'NONE', #12291 ) ;
#6063 = CARTESIAN_POINT ( 'NONE',  ( 35.00000000000000000, 90.00000000000000000, 6.000000000000000000 ) ) ;
#6064 = ORIENTED_EDGE ( 'NONE', *, *, #12198, .F. ) ;
#6065 = DIRECTION ( 'NONE',  ( 0.000000000000000000, -1.000000000000000000, 0.000000000000000000 ) ) ;
#6066 = VERTEX_POINT ( 'NONE', #2483 ) ;
#6067 = EDGE_CURVE ( 'NONE', #6209, #11848, #497, .T. ) ;
#6068 = EDGE_CURVE ( 'NONE', #571, #8179, #6437, .T. ) ;
#6069 = DIRECTION ( 'NONE',  ( -1.000000000000000000, -5.551115123125781124E-15, 0.000000000000000000 ) ) ;
#6070 = VECTOR ( 'NONE', #12058, 1000.000000000000000 ) ;
#6071 = LINE ( 'NONE', #8953, #2903 ) ;
#6072 = VERTEX_POINT ( 'NONE', #4638 ) ;
#6073 =( BOUNDED_CURVE ( )  B_SPLINE_CURVE ( 2, ( #9840, #7812, #5974, #12788, #3769, #9969, #6765 ),
 .UNSPECIFIED., .F., .F. ) 
 B_SPLINE_CURVE_WITH_KNOTS ( ( 3, 2, 2, 3 ),
 ( 0.3999999999999999667, 0.4333333333333333481, 0.4666666666666667296, 0.5000000000000001110 ),
 .UNSPECIFIED. ) 
 CURVE ( )  GEOMETRIC_REPRESENTATION_ITEM ( )  RATIONAL_B_SPLINE_CURVE ( ( 1.000000000000000444, 0.8660254037844385966, 1.000000000000000000, 0.8660254037844387076, 1.000000000000000000, 0.8660254037844382635, 1.000000000000000444 ) ) 
 REPRESENTATION_ITEM ( '' )  );
#6074 = EDGE_LOOP ( 'NONE', ( #7842, #495, #10728, #11018 ) ) ;
#6075 = PLANE ( 'NONE',  #5755 ) ;
#6076 = EDGE_LOOP ( 'NONE', ( #10405, #5627, #6929, #10969 ) ) ;
#6077 = APPLICATION_PROTOCOL_DEFINITION ( 'draft international standard', 'automotive_design', 1998, #6833 ) ;
#6078 = CARTESIAN_POINT ( 'NONE',  ( 66.44356964374999563, 90.00000000000000000, 3.228125000614517237 ) ) ;
#6079 = EDGE_LOOP ( 'NONE', ( #2956, #10660, #2480 ) ) ;
#6080 = VECTOR ( 'NONE', #6281, 1000.000000000000227 ) ;
#6081 = DIRECTION ( 'NONE',  ( 0.000000000000000000, 0.000000000000000000, 1.000000000000000000 ) ) ;
#6082 = EDGE_LOOP ( 'NONE', ( #12567, #11047 ) ) ;
#6083 = LINE ( 'NONE', #8236, #12145 ) ;
#6084 = DIRECTION ( 'NONE',  ( -0.000000000000000000, -1.000000000000000000, -0.000000000000000000 ) ) ;
#6085 = DIRECTION ( 'NONE',  ( -1.000000000000000000, 0.000000000000000000, 0.000000000000000000 ) ) ;
#6086 =( REPRESENTATION_RELATIONSHIP ('NONE','NONE', #1997, #4597 ) REPRESENTATION_RELATIONSHIP_WITH_TRANSFORMATION ( #6532 )SHAPE_REPRESENTATION_RELATIONSHIP( ) );
#6087 = CARTESIAN_POINT ( 'NONE',  ( 1.040000000000000036, 0.8660254037844390407, -0.5000000000000002220 ) ) ;
#6088 = EDGE_CURVE ( 'NONE', #4781, #7005, #7640, .T. ) ;
#6089 = ORIENTED_EDGE ( 'NONE', *, *, #244, .T. ) ;
#6090 = CARTESIAN_POINT ( 'NONE',  ( 66.44356964374999563, 71.84604660189820891, 4.596875000614517148 ) ) ;
#6091 = CARTESIAN_POINT ( 'NONE',  ( -4.270088556250601699E-16, 30.00000000000000000, 8.000000000000000000 ) ) ;
#6092 = CARTESIAN_POINT ( 'NONE',  ( 40.89629752784551897, 120.7937367018730725, 3.000000000000000000 ) ) ;
#6093 = VERTEX_POINT ( 'NONE', #11630 ) ;
#6094 = LINE ( 'NONE', #11263, #4875 ) ;
#6095 = ORIENTED_EDGE ( 'NONE', *, *, #8035, .F. ) ;
#6096 = VECTOR ( 'NONE', #6282, 1000.000000000000000 ) ;
#6097 = DIRECTION ( 'NONE',  ( -0.000000000000000000, -0.000000000000000000, -1.000000000000000000 ) ) ;
#6098 = CARTESIAN_POINT ( 'NONE',  ( 3.556430356250015024, 90.00000000000000000, 4.803125000614516971 ) ) ;
#6099 = ORIENTED_EDGE ( 'NONE', *, *, #3712, .F. ) ;
#6100 = CARTESIAN_POINT ( 'NONE',  ( 50.72178482187499071, 117.2309300971526937, 3.809375000614517504 ) ) ;
#6101 = CARTESIAN_POINT ( 'NONE',  ( -60.00000000000000000, 30.00000000000000000, -10.00000000000000355 ) ) ;
#6102 = DIRECTION ( 'NONE',  ( -0.5000000000000045519, 0.8660254037844360431, 0.000000000000000000 ) ) ;
#6103 = EDGE_CURVE ( 'NONE', #2940, #9627, #10647, .T. ) ;
#6104 = AXIS2_PLACEMENT_3D ( 'NONE', #5221, #430, #11299 ) ;
#6105 = DIRECTION ( 'NONE',  ( 0.000000000000000000, 0.000000000000000000, -1.000000000000000000 ) ) ;
#6106 = FACE_OUTER_BOUND ( 'NONE', #4650, .T. ) ;
#6107 = LINE ( 'NONE', #11213, #1338 ) ;
#6108 = CARTESIAN_POINT ( 'NONE',  ( 25.83484861008832567, 86.00000000000000000, -18.00000000000000355 ) ) ;
#6109 = CYLINDRICAL_SURFACE ( 'NONE', #624, 1.599999999999990319 ) ;
#6110 = CYLINDRICAL_SURFACE ( 'NONE', #540, 2.849999999999999201 ) ;
#6111 = ORIENTED_EDGE ( 'NONE', *, *, #8827, .T. ) ;
#6112 = LINE ( 'NONE', #9193, #4749 ) ;
#6113 = ORIENTED_EDGE ( 'NONE', *, *, #9318, .F. ) ;
#6114 = EDGE_CURVE ( 'NONE', #10261, #8136, #692, .T. ) ;
#6115 = CIRCLE ( 'NONE', #3835, 31.20000000000000284 ) ;
#6116 = CARTESIAN_POINT ( 'NONE',  ( -56.80384757729341771, 34.46410161513777837, 0.000000000000000000 ) ) ;
#6117 = CARTESIAN_POINT ( 'NONE',  ( -38.66666666666665719, 2.000000000000000000, -7.999999999999996447 ) ) ;
#6118 = CARTESIAN_POINT ( 'NONE',  ( 31.50000000000000000, 90.00000000000000000, 6.000000000000000000 ) ) ;
#6119 = ORIENTED_EDGE ( 'NONE', *, *, #7874, .T. ) ;
#6120 = CARTESIAN_POINT ( 'NONE',  ( 21.49999999999998579, 90.00000000000000000, -10.00000000000000178 ) ) ;
#6121 = LINE ( 'NONE', #10185, #5008 ) ;
#6122 = EDGE_LOOP ( 'NONE', ( #9284, #1495, #12007, #6640 ) ) ;
#6123 = CIRCLE ( 'NONE', #7605, 10.00000000000000178 ) ;
#6124 = ORIENTED_EDGE ( 'NONE', *, *, #4550, .F. ) ;
#6125 = DIRECTION ( 'NONE',  ( -1.000000000000000000, 0.000000000000000000, -2.891205793294679312E-17 ) ) ;
#6126 = ORIENTED_EDGE ( 'NONE', *, *, #10746, .F. ) ;
#6127 = EDGE_CURVE ( 'NONE', #5561, #10542, #6040, .T. ) ;
#6128 = FACE_BOUND ( 'NONE', #7571, .T. ) ;
#6129 = PRODUCT_DEFINITION_FORMATION_WITH_SPECIFIED_SOURCE ( 'ANY', '', #1451, .NOT_KNOWN. ) ;
#6130 = LINE ( 'NONE', #3208, #12919 ) ;
#6131 = ORIENTED_EDGE ( 'NONE', *, *, #1902, .F. ) ;
#6132 = TOROIDAL_SURFACE ( 'NONE', #713, 1.599999999999998757, 0.1000000000000000056 ) ;
#6133 = ORIENTED_EDGE ( 'NONE', *, *, #7308, .T. ) ;
#6134 = FACE_OUTER_BOUND ( 'NONE', #10601, .T. ) ;
#6135 = ORIENTED_EDGE ( 'NONE', *, *, #8244, .T. ) ;
#6136 = SHAPE_DEFINITION_REPRESENTATION ( #9283, #1066 ) ;
#6137 = CARTESIAN_POINT ( 'NONE',  ( 50.59999999999999432, 117.0199925980744666, 4.512500001229033941 ) ) ;
#6138 = ADVANCED_FACE ( 'NONE', ( #7765 ), #8689, .T. ) ;
#6139 = EDGE_LOOP ( 'NONE', ( #8446, #1686, #9060, #1035, #372, #11283 ) ) ;
#6140 = FACE_BOUND ( 'NONE', #2478, .T. ) ;
#6141 = DIRECTION ( 'NONE',  ( 5.624500927088228034E-17, -1.370729058197317775E-18, -1.000000000000000000 ) ) ;
#6142 = ORIENTED_EDGE ( 'NONE', *, *, #10903, .F. ) ;
#6143 = DIRECTION ( 'NONE',  ( -0.000000000000000000, -1.000000000000000000, -0.000000000000000000 ) ) ;
#6144 = AXIS2_PLACEMENT_3D ( 'NONE', #10933, #1985, #8848 ) ;
#6145 = CARTESIAN_POINT ( 'NONE',  ( 66.44356964374998142, 108.1539533981018053, 4.615625000614516971 ) ) ;
#6146 = VECTOR ( 'NONE', #6301, 1000.000000000000000 ) ;
#6147 = CARTESIAN_POINT ( 'NONE',  ( 41.31805916882747454, 91.52713075379783447, 4.000000000000000000 ) ) ;
#6148 =( BOUNDED_SURFACE ( )  B_SPLINE_SURFACE ( 1, 2, ( 
 ( #4539, #9635, #662, #1457, #9438, #3628, #11332, #4470, #2514, #6491, #10486, #1521, #5510, #8532, #8841, #3947, #7796, #6942, #982, #3754, #5955, #1721, #916, #4920, #7930, #8656, #1910, #10740, #8781, #8906, #12711, #8718, #12774, #2710, #7736, #9825, #10926, #6685, #4793, #852, #2961, #12652, #3693, #6811, #12836, #5708, #3884, #10866, #11853, #7673, #9763, #7863, #2901, #11660, #12902 ),
 ( #9695, #5834, #11790, #789, #5892, #2774, #730, #9884, #4732, #6746, #6878, #11724, #1784, #4857, #11916, #10681, #5772, #1978, #9953, #3816, #2836, #10807, #1849, #2109, #9031, #8967, #4266, #11977, #3224, #5104, #8255, #12245, #3159, #122, #4980, #3292, #12111, #2309, #10016, #3023, #11254, #4138, #1249, #8189, #8126, #11192, #5935, #10143, #4010, #4073, #7010, #6221, #10274, #7993, #7137 ) ),
 .UNSPECIFIED., .F., .F., .F. ) 
 B_SPLINE_SURFACE_WITH_KNOTS ( ( 2, 2 ),
 ( 3, 2, 2, 2, 2, 2, 2, 2, 2, 2, 2, 2, 2, 2, 2, 2, 2, 2, 2, 2, 2, 2, 2, 2, 2, 2, 2, 3 ),
 ( 0.000000000000000000, 1.000000000000000000 ),
 ( 0.000000000000000000, 0.03333333333333333287, 0.06666666666666666574, 0.1000000000000000056, 0.1333333333333333315, 0.1666666666666666574, 0.2000000000000000111, 0.2333333333333333370, 0.2666666666666666630, 0.2999999999999999889, 0.3333333333333333148, 0.3666666666666666408, 0.4000000000000000222, 0.4333333333333333481, 0.4666666666666666741, 0.5000000000000000000, 0.5333333333333333259, 0.5666666666666666519, 0.5999999999999999778, 0.6333333333333333037, 0.6666666666666666297, 0.6999999999999999556, 0.7333333333333332815, 0.7666666666666667185, 0.8000000000000000444, 0.8333333333333333703, 0.8666666666666666963, 0.8887752010635167066 ),
 .UNSPECIFIED. ) 
 GEOMETRIC_REPRESENTATION_ITEM ( )  RATIONAL_B_SPLINE_SURFACE ( (
 ( 1.000000000000000000, 0.8660254037844387076, 1.000000000000000000, 0.8660254037844387076, 1.000000000000000000, 0.8660254037844387076, 1.000000000000000000, 0.8660254037844387076, 1.000000000000000000, 0.8660254037844387076, 1.000000000000000000, 0.8660254037844387076, 1.000000000000000000, 0.8660254037844387076, 1.000000000000000000, 0.8660254037844387076, 1.000000000000000000, 0.8660254037844387076, 1.000000000000000000, 0.8660254037844387076, 1.000000000000000000, 0.8660254037844387076, 1.000000000000000000, 0.8660254037844387076, 1.000000000000000000, 0.8660254037844387076, 1.000000000000000000, 0.8660254037844387076, 1.000000000000000000, 0.8660254037844387076, 1.000000000000000000, 0.8660254037844387076, 1.000000000000000000, 0.8660254037844387076, 1.000000000000000000, 0.8660254037844387076, 1.000000000000000000, 0.8660254037844387076, 1.000000000000000000, 0.8660254037844387076, 1.000000000000000000, 0.8660254037844387076, 1.000000000000000000, 0.8660254037844387076, 1.000000000000000000, 0.8660254037844387076, 1.000000000000000000, 0.8660254037844387076, 1.000000000000000000, 0.8660254037844387076, 1.000000000000000000, 0.8660254037844387076, 1.000000000000000000, 0.9111405409379251807, 0.9401542263054123438),
 ( 1.000000000000000000, 0.8660254037844387076, 1.000000000000000000, 0.8660254037844387076, 1.000000000000000000, 0.8660254037844387076, 1.000000000000000000, 0.8660254037844387076, 1.000000000000000000, 0.8660254037844387076, 1.000000000000000000, 0.8660254037844387076, 1.000000000000000000, 0.8660254037844387076, 1.000000000000000000, 0.8660254037844387076, 1.000000000000000000, 0.8660254037844387076, 1.000000000000000000, 0.8660254037844387076, 1.000000000000000000, 0.8660254037844387076, 1.000000000000000000, 0.8660254037844387076, 1.000000000000000000, 0.8660254037844387076, 1.000000000000000000, 0.8660254037844387076, 1.000000000000000000, 0.8660254037844387076, 1.000000000000000000, 0.8660254037844387076, 1.000000000000000000, 0.8660254037844387076, 1.000000000000000000, 0.8660254037844387076, 1.000000000000000000, 0.8660254037844387076, 1.000000000000000000, 0.8660254037844387076, 1.000000000000000000, 0.8660254037844387076, 1.000000000000000000, 0.8660254037844387076, 1.000000000000000000, 0.8660254037844387076, 1.000000000000000000, 0.8660254037844387076, 1.000000000000000000, 0.8660254037844387076, 1.000000000000000000, 0.8660254037844387076, 1.000000000000000000, 0.9111405409379251807, 0.9401542263054123438) ) ) 
 REPRESENTATION_ITEM ( '' )  SURFACE ( )  );
#6149 = CYLINDRICAL_SURFACE ( 'NONE', #8537, 2.396199811936270407 ) ;
#6150 = EDGE_CURVE ( 'NONE', #1892, #5455, #12802, .T. ) ;
#6151 = FILL_AREA_STYLE ('',( #10991 ) ) ;
#6152 = FACE_OUTER_BOUND ( 'NONE', #4124, .T. ) ;
#6153 = EDGE_LOOP ( 'NONE', ( #924, #3801, #7341, #5591 ) ) ;
#6154 = CARTESIAN_POINT ( 'NONE',  ( 66.19999999999998863, 90.00000000000000000, 4.325000000000000178 ) ) ;
#6155 = ORIENTED_EDGE ( 'NONE', *, *, #6631, .T. ) ;
#6156 = CIRCLE ( 'NONE', #5123, 3.500000000000003109 ) ;
#6157 = CARTESIAN_POINT ( 'NONE',  ( 50.00000000000000000, 0.000000000000000000, 10.00000000000000000 ) ) ;
#6158 = CARTESIAN_POINT ( 'NONE',  ( 46.98957880828161393, 117.5000000000000711, -3.000000000000000000 ) ) ;
#6159 = VERTEX_POINT ( 'NONE', #1065 ) ;
#6160 = ADVANCED_FACE ( 'NONE', ( #3848 ), #3721, .T. ) ;
#6161 = VECTOR ( 'NONE', #3806, 1000.000000000000227 ) ;
#6162 = FACE_OUTER_BOUND ( 'NONE', #8558, .T. ) ;
#6163 = EDGE_LOOP ( 'NONE', ( #3407, #7657, #9803, #10497 ) ) ;
#6164 = CARTESIAN_POINT ( 'NONE',  ( 48.49999999999995737, 90.00000000000000000, -5.000000000000000000 ) ) ;
#6165 = UNCERTAINTY_MEASURE_WITH_UNIT (LENGTH_MEASURE( 1.000000000000000082E-05 ), #7994, 'distance_accuracy_value', 'NONE');
#6166 = CARTESIAN_POINT ( 'NONE',  ( 35.00000000000000711, 53.69209320379640360, 3.115625000614517415 ) ) ;
#6167 = ORIENTED_EDGE ( 'NONE', *, *, #1120, .T. ) ;
#6168 = CARTESIAN_POINT ( 'NONE',  ( 64.31840934454761793, 100.6710296366163249, 2.999476389609550431 ) ) ;
#6169 = CARTESIAN_POINT ( 'NONE',  ( -65.00000000000004263, 38.66025403784436065, 3.000000000000000000 ) ) ;
#6170 = APPLICATION_CONTEXT ( 'automotive_design' ) ;
#6171 = AXIS2_PLACEMENT_3D ( 'NONE', #3701, #8664, #2523 ) ;
#6172 = FACE_OUTER_BOUND ( 'NONE', #5392, .T. ) ;
#6173 =( GEOMETRIC_REPRESENTATION_CONTEXT ( 3 ) GLOBAL_UNCERTAINTY_ASSIGNED_CONTEXT ( ( #12082 ) ) GLOBAL_UNIT_ASSIGNED_CONTEXT ( ( #7526, #9616, #6663 ) ) REPRESENTATION_CONTEXT ( 'NONE', 'WORKASPACE' ) );
#6174 = CARTESIAN_POINT ( 'NONE',  ( 1.617350269189632428, 0.000000000000000000, 0.000000000000000000 ) ) ;
#6175 = LINE ( 'NONE', #3182, #5311 ) ;
#6176 = PRODUCT_RELATED_PRODUCT_CATEGORY ( 'part', '', ( #5413 ) ) ;
#6177 = VECTOR ( 'NONE', #9908, 1000.000000000000114 ) ;
#6178 = CARTESIAN_POINT ( 'NONE',  ( -4.338286831716297698, 0.4117131682837010809, -0.8000000000000000444 ) ) ;
#6179 = CIRCLE ( 'NONE', #10150, 10.00000000000000178 ) ;
#6180 = DIRECTION ( 'NONE',  ( 0.000000000000000000, -1.000000000000000000, 0.000000000000000000 ) ) ;
#6181 = CARTESIAN_POINT ( 'NONE',  ( 2.179634403564814971, -5.614030811971695734, 0.000000000000000000 ) ) ;
#6182 = ADVANCED_FACE ( 'NONE', ( #6781 ), #11008, .F. ) ;
#6183 = ORIENTED_EDGE ( 'NONE', *, *, #9652, .T. ) ;
#6184 = CARTESIAN_POINT ( 'NONE',  ( 7.500000000000000000, 30.00000000000000000, 0.000000000000000000 ) ) ;
#6185 = ORIENTED_EDGE ( 'NONE', *, *, #8234, .F. ) ;
#6186 = AXIS2_PLACEMENT_3D ( 'NONE', #3638, #11343, #2586 ) ;
#6187 = CARTESIAN_POINT ( 'NONE',  ( 35.75000000000000711, 92.49999999999998579, 6.000000000000000000 ) ) ;
#6188 = CARTESIAN_POINT ( 'NONE',  ( 66.20000000000008811, 108.0133283987162542, 4.025000001229034119 ) ) ;
#6189 = CARTESIAN_POINT ( 'NONE',  ( -6.666666666666660745, -5.000000000000000000, 1.499999999999999556 ) ) ;
#6190 = UNCERTAINTY_MEASURE_WITH_UNIT (LENGTH_MEASURE( 1.000000000000000082E-05 ), #7461, 'distance_accuracy_value', 'NONE');
#6191 = EDGE_LOOP ( 'NONE', ( #7976, #11412, #456, #8443 ) ) ;
#6192 = DIRECTION ( 'NONE',  ( 1.000000000000000000, 0.000000000000000000, -0.000000000000000000 ) ) ;
#6193 = DIRECTION ( 'NONE',  ( -1.000000000000000000, 0.000000000000000000, 0.000000000000000000 ) ) ;
#6194 = EDGE_CURVE ( 'NONE', #1830, #12152, #9606, .T. ) ;
#6195 = VERTEX_POINT ( 'NONE', #5675 ) ;
#6196 = DIRECTION ( 'NONE',  ( -0.8660254037844394848, -0.4999999999999984457, -0.000000000000000000 ) ) ;
#6197 = ADVANCED_FACE ( 'NONE', ( #8747 ), #11565, .T. ) ;
#6198 = ORIENTED_EDGE ( 'NONE', *, *, #9520, .T. ) ;
#6199 = CIRCLE ( 'NONE', #2662, 1.219500000000000028 ) ;
#6200 = LINE ( 'NONE', #7621, #10695 ) ;
#6201 = VERTEX_POINT ( 'NONE', #11690 ) ;
#6202 = DIRECTION ( 'NONE',  ( 0.000000000000000000, 1.000000000000000000, 0.000000000000000000 ) ) ;
#6203 = DIRECTION ( 'NONE',  ( 0.000000000000000000, 0.000000000000000000, 1.000000000000000000 ) ) ;
#6204 = VERTEX_POINT ( 'NONE', #2741 ) ;
#6205 = PRODUCT_DEFINITION_CONTEXT ( 'detailed design', #8533, 'design' ) ;
#6206 = ORIENTED_EDGE ( 'NONE', *, *, #11997, .F. ) ;
#6207 = AXIS2_PLACEMENT_3D ( 'NONE', #10585, #10644, #4633 ) ;
#6208 = CARTESIAN_POINT ( 'NONE',  ( 77.59086064835547347, 64.09101861717452664, 1.000000000000003109 ) ) ;
#6209 = VERTEX_POINT ( 'NONE', #7028 ) ;
#6210 = CARTESIAN_POINT ( 'NONE',  ( -48.33333333333332860, 3.649999999999999911, -1.734723475976807094E-15 ) ) ;
#6211 = CARTESIAN_POINT ( 'NONE',  ( 35.00000000000000711, 53.69209320379640360, 4.015625000614517326 ) ) ;
#6212 = ADVANCED_FACE ( 'NONE', ( #6716 ), #631, .T. ) ;
#6213 = ORIENTED_EDGE ( 'NONE', *, *, #917, .T. ) ;
#6214 = CARTESIAN_POINT ( 'NONE',  ( 25.00000000000000355, 2.000000000000000000, -5.750000000000000000 ) ) ;
#6215 = DIRECTION ( 'NONE',  ( 0.000000000000000000, 0.000000000000000000, -1.000000000000000000 ) ) ;
#6216 = ORIENTED_EDGE ( 'NONE', *, *, #1524, .T. ) ;
#6217 = CARTESIAN_POINT ( 'NONE',  ( -60.00000000000000000, 30.00000000000000000, 0.9999999999999926725 ) ) ;
#6218 = CARTESIAN_POINT ( 'NONE',  ( 50.72178482187501203, 62.76906990284730625, 3.603125000614517681 ) ) ;
#6219 = CIRCLE ( 'NONE', #7892, 1.500000000000001332 ) ;
#6220 = CARTESIAN_POINT ( 'NONE',  ( 66.19999999999998863, 90.00000000000000000, 3.087500001229034119 ) ) ;
#6221 = CARTESIAN_POINT ( 'NONE',  ( 35.00000000000000000, 126.0266567974326222, 2.750000001229033764 ) ) ;
#6222 =( LENGTH_UNIT ( ) NAMED_UNIT ( * ) SI_UNIT ( .MILLI., .METRE. ) );
#6223 = LINE ( 'NONE', #4140, #10849 ) ;
#6224 = ORIENTED_EDGE ( 'NONE', *, *, #6068, .F. ) ;
#6225 = CARTESIAN_POINT ( 'NONE',  ( 3.800000000000015365, 108.0133283987163111, 4.512500000000000178 ) ) ;
#6226 = VERTEX_POINT ( 'NONE', #2061 ) ;
#6227 = AXIS2_PLACEMENT_3D ( 'NONE', #3388, #219, #352 ) ;
#6228 = CARTESIAN_POINT ( 'NONE',  ( 7.500000000000000000, 30.00000000000000000, 0.000000000000000000 ) ) ;
#6229 = EDGE_CURVE ( 'NONE', #8130, #10434, #6869, .T. ) ;
#6230 = AXIS2_PLACEMENT_3D ( 'NONE', #9098, #7206, #7332 ) ;
#6231 = ORIENTED_EDGE ( 'NONE', *, *, #1962, .F. ) ;
#6232 = CARTESIAN_POINT ( 'NONE',  ( 35.00000000000000711, 53.97334320256736362, 3.762500000000000178 ) ) ;
#6233 = ORIENTED_EDGE ( 'NONE', *, *, #5131, .F. ) ;
#6234 = DIRECTION ( 'NONE',  ( 0.000000000000000000, 0.5000000000000003331, -0.8660254037844384856 ) ) ;
#6235 = CARTESIAN_POINT ( 'NONE',  ( 50.72178482187501203, 62.76906990284730625, 4.053125000614517859 ) ) ;
#6236 = CARTESIAN_POINT ( 'NONE',  ( 35.00000000000000711, 53.69209320379639649, 4.071875000614516793 ) ) ;
#6237 = CARTESIAN_POINT ( 'NONE',  ( 45.00000000000000000, 0.000000000000000000, -5.750000000000000000 ) ) ;
#6238 = ADVANCED_FACE ( 'NONE', ( #5613 ), #9728, .F. ) ;
#6239 = CYLINDRICAL_SURFACE ( 'NONE', #600, 3.500000000000003109 ) ;
#6240 = ADVANCED_FACE ( 'NONE', ( #3784, #10774, #4825, #3310, #8079, #75, #12325 ), #2262, .F. ) ;
#6241 = DIRECTION ( 'NONE',  ( 1.000000000000000000, 0.000000000000000000, 0.000000000000000000 ) ) ;
#6242 = LINE ( 'NONE', #6624, #4170 ) ;
#6243 = LINE ( 'NONE', #5196, #6353 ) ;
#6244 = DIRECTION ( 'NONE',  ( -0.000000000000000000, -1.000000000000000000, -0.000000000000000000 ) ) ;
#6245 = CARTESIAN_POINT ( 'NONE',  ( 44.16515138991168499, 86.00000000000000000, -8.000000000000000000 ) ) ;
#6246 = CARTESIAN_POINT ( 'NONE',  ( 3.556430356250015024, 90.00000000000000000, 3.059375000614517059 ) ) ;
#6247 = VERTEX_POINT ( 'NONE', #10292 ) ;
#6248 = DIRECTION ( 'NONE',  ( 0.000000000000000000, 0.000000000000000000, -1.000000000000000000 ) ) ;
#6249 = ORIENTED_EDGE ( 'NONE', *, *, #7392, .F. ) ;
#6250 = AXIS2_PLACEMENT_3D ( 'NONE', #3555, #522, #9366 ) ;
#6251 = VECTOR ( 'NONE', #2304, 1000.000000000000000 ) ;
#6252 = CARTESIAN_POINT ( 'NONE',  ( 4.270088556250601699E-16, 2.000000000000000000, -8.000000000000000000 ) ) ;
#6253 = CARTESIAN_POINT ( 'NONE',  ( 19.40000000000000924, 117.0199925980744666, 4.137500001229033941 ) ) ;
#6254 = EDGE_CURVE ( 'NONE', #7039, #9204, #7093, .T. ) ;
#6255 = CARTESIAN_POINT ( 'NONE',  ( 8.999999999999987566, 72.14656965084313356, 3.000000000000000000 ) ) ;
#6256 = ORIENTED_EDGE ( 'NONE', *, *, #9643, .T. ) ;
#6257 = DIRECTION ( 'NONE',  ( -1.000000000000000000, 0.000000000000000000, 0.000000000000000000 ) ) ;
#6258 = CARTESIAN_POINT ( 'NONE',  ( -36.66666666666665009, 46.12451549659709116, -7.999999999999996447 ) ) ;
#6259 = VERTEX_POINT ( 'NONE', #9245 ) ;
#6260 = AXIS2_PLACEMENT_3D ( 'NONE', #3394, #5341, #6513 ) ;
#6261 = DIRECTION ( 'NONE',  ( 0.000000000000000000, 0.000000000000000000, 1.000000000000000000 ) ) ;
#6262 = CARTESIAN_POINT ( 'NONE',  ( 21.49999999999998579, 94.00000000000000000, -10.00000000000000000 ) ) ;
#6263 = ORIENTED_EDGE ( 'NONE', *, *, #3837, .F. ) ;
#6264 =( REPRESENTATION_RELATIONSHIP ('NONE','NONE', #1997, #9523 ) REPRESENTATION_RELATIONSHIP_WITH_TRANSFORMATION ( #6854 )SHAPE_REPRESENTATION_RELATIONSHIP( ) );
#6265 = ORIENTED_EDGE ( 'NONE', *, *, #2587, .T. ) ;
#6266 = CARTESIAN_POINT ( 'NONE',  ( 25.00000000000000000, 90.00000000000000000, -18.00000000000000355 ) ) ;
#6267 = LINE ( 'NONE', #11366, #7697 ) ;
#6268 = EDGE_CURVE ( 'NONE', #12120, #716, #7287, .T. ) ;
#6269 = ORIENTED_EDGE ( 'NONE', *, *, #7598, .F. ) ;
#6270 = VECTOR ( 'NONE', #7162, 1000.000000000000000 ) ;
#6271 = ADVANCED_FACE ( 'NONE', ( #7154 ), #6239, .T. ) ;
#6272 = VERTEX_POINT ( 'NONE', #6300 ) ;
#6273 = CARTESIAN_POINT ( 'NONE',  ( 0.000000000000000000, -0.5773502691896253980, -1.000000000000000000 ) ) ;
#6274 = ORIENTED_EDGE ( 'NONE', *, *, #5865, .F. ) ;
#6275 = CARTESIAN_POINT ( 'NONE',  ( 48.49999999999995737, 90.00000000000000000, -11.64999999999999680 ) ) ;
#6276 = CARTESIAN_POINT ( 'NONE',  ( 3.556430356250028790, 71.84604660189818048, 3.040625000614517237 ) ) ;
#6277 = ORIENTED_EDGE ( 'NONE', *, *, #4432, .T. ) ;
#6278 = CARTESIAN_POINT ( 'NONE',  ( -38.66666666666665719, 46.12451549659709116, 7.999999999999996447 ) ) ;
#6279 = VERTEX_POINT ( 'NONE', #11273 ) ;
#6280 = AXIS2_PLACEMENT_3D ( 'NONE', #3637, #6565, #2782 ) ;
#6281 = DIRECTION ( 'NONE',  ( -0.000000000000000000, -0.5000000000000000000, 0.8660254037844385966 ) ) ;
#6282 = DIRECTION ( 'NONE',  ( 1.000000000000000000, 0.000000000000000000, 0.000000000000000000 ) ) ;
#6283 = CARTESIAN_POINT ( 'NONE',  ( 35.00000000000000000, 90.00000000000000000, 4.800000000000000711 ) ) ;
#6284 = ADVANCED_FACE ( 'NONE', ( #6172 ), #8207, .T. ) ;
#6285 = DIRECTION ( 'NONE',  ( 0.000000000000000000, 0.000000000000000000, -1.000000000000000000 ) ) ;
#6286 = EDGE_LOOP ( 'NONE', ( #11364, #5278 ) ) ;
#6287 = AXIS2_PLACEMENT_3D ( 'NONE', #6743, #10735, #9503 ) ;
#6288 = CARTESIAN_POINT ( 'NONE',  ( 3.556430356250028790, 71.84604660189818048, 4.446875000614517681 ) ) ;
#6289 = ORIENTED_EDGE ( 'NONE', *, *, #653, .F. ) ;
#6290 = FACE_OUTER_BOUND ( 'NONE', #3955, .T. ) ;
#6291 = ORIENTED_EDGE ( 'NONE', *, *, #4050, .F. ) ;
#6292 = DIRECTION ( 'NONE',  ( 0.000000000000000000, 0.000000000000000000, 1.000000000000000000 ) ) ;
#6293 = ORIENTED_EDGE ( 'NONE', *, *, #310, .F. ) ;
#6294 = DIRECTION ( 'NONE',  ( -1.000000000000000000, 0.000000000000000000, 0.000000000000000000 ) ) ;
#6295 = CARTESIAN_POINT ( 'NONE',  ( 0.000000000000000000, -1.154700538379251240, 1.014316938424154191E-17 ) ) ;
#6296 = LINE ( 'NONE', #5318, #11537 ) ;
#6297 = CIRCLE ( 'NONE', #218, 31.20000000000000639 ) ;
#6298 = DIRECTION ( 'NONE',  ( 0.000000000000000000, 0.000000000000000000, 1.000000000000000000 ) ) ;
#6299 = ADVANCED_FACE ( 'NONE', ( #2385 ), #5191, .F. ) ;
#6300 = CARTESIAN_POINT ( 'NONE',  ( 13.95244456248789788, 109.9499476216067819, 1.000000000000003109 ) ) ;
#6301 = DIRECTION ( 'NONE',  ( 0.000000000000000000, 0.000000000000000000, 1.000000000000000000 ) ) ;
#6302 = CARTESIAN_POINT ( 'NONE',  ( 23.09999999999997300, 90.00000000000000000, -8.000000000000000000 ) ) ;
#6303 = DIRECTION ( 'NONE',  ( 0.000000000000000000, 0.000000000000000000, 1.000000000000000000 ) ) ;
#6304 = VECTOR ( 'NONE', #6125, 1000.000000000000000 ) ;
#6305 = DIRECTION ( 'NONE',  ( -0.000000000000000000, -0.000000000000000000, 1.000000000000000000 ) ) ;
#6306 = EDGE_CURVE ( 'NONE', #4911, #571, #5614, .T. ) ;
#6307 = EDGE_CURVE ( 'NONE', #8177, #4318, #5320, .T. ) ;
#6308 = LINE ( 'NONE', #1530, #10242 ) ;
#6309 = CARTESIAN_POINT ( 'NONE',  ( 50.72178482187501203, 62.76906990284730625, 3.659375000614517592 ) ) ;
#6310 = ORIENTED_EDGE ( 'NONE', *, *, #2455, .F. ) ;
#6311 = CARTESIAN_POINT ( 'NONE',  ( 1.040000000000000036, -1.154700538379251684, 0.000000000000000000 ) ) ;
#6312 = ORIENTED_EDGE ( 'NONE', *, *, #10407, .F. ) ;
#6313 = AXIS2_PLACEMENT_3D ( 'NONE', #11270, #12191, #3241 ) ;
#6314 = ADVANCED_FACE ( 'NONE', ( #4092 ), #12065, .T. ) ;
#6315 = DIRECTION ( 'NONE',  ( -0.000000000000000000, -0.000000000000000000, -1.000000000000000000 ) ) ;
#6316 = DIRECTION ( 'NONE',  ( -0.5000000000000036637, 0.8660254037844365982, 0.000000000000000000 ) ) ;
#6317 = LINE ( 'NONE', #6255, #12410 ) ;
#6318 = ORIENTED_EDGE ( 'NONE', *, *, #11009, .F. ) ;
#6319 = DIRECTION ( 'NONE',  ( 1.000000000000000000, 0.000000000000000000, 0.000000000000000000 ) ) ;
#6320 = CYLINDRICAL_SURFACE ( 'NONE', #5851, 1.500000000000001332 ) ;
#6321 = ORIENTED_EDGE ( 'NONE', *, *, #12182, .F. ) ;
#6322 = VECTOR ( 'NONE', #1554, 1000.000000000000000 ) ;
#6323 = CARTESIAN_POINT ( 'NONE',  ( 35.75000000000000711, 92.49999999999998579, -4.802775637732004554 ) ) ;
#6324 = ORIENTED_EDGE ( 'NONE', *, *, #7958, .F. ) ;
#6325 = VERTEX_POINT ( 'NONE', #2126 ) ;
#6326 = EDGE_CURVE ( 'NONE', #1744, #12575, #9591, .T. ) ;
#6327 = PLANE ( 'NONE',  #3824 ) ;
#6328 = LINE ( 'NONE', #8305, #12294 ) ;
#6329 = VERTEX_POINT ( 'NONE', #9313 ) ;
#6330 = ORIENTED_EDGE ( 'NONE', *, *, #390, .T. ) ;
#6331 = LINE ( 'NONE', #1299, #12230 ) ;
#6332 = ORIENTED_EDGE ( 'NONE', *, *, #6543, .T. ) ;
#6333 = AXIS2_PLACEMENT_3D ( 'NONE', #243, #1040, #1105 ) ;
#6334 = APPLICATION_PROTOCOL_DEFINITION ( 'draft international standard', 'automotive_design', 1998, #4174 ) ;
#6335 = CARTESIAN_POINT ( 'NONE',  ( 35.00000000000000000, 126.0266567974326222, 2.750000001229033764 ) ) ;
#6336 = VERTEX_POINT ( 'NONE', #9116 ) ;
#6337 = DIRECTION ( 'NONE',  ( -0.000000000000000000, -1.000000000000000000, -0.000000000000000000 ) ) ;
#6338 = VERTEX_POINT ( 'NONE', #12132 ) ;
#6339 = PRESENTATION_LAYER_ASSIGNMENT (  '', '', ( #1959 ) ) ;
#6340 =( BOUNDED_CURVE ( )  B_SPLINE_CURVE ( 2, ( #6876, #8125, #7862, #8965, #11852, #1909, #5890 ),
 .UNSPECIFIED., .F., .F. ) 
 B_SPLINE_CURVE_WITH_KNOTS ( ( 3, 2, 2, 3 ),
 ( 0.5000000000000001110, 0.5333333333333334370, 0.5666666666666666519, 0.5999999999999999778 ),
 .UNSPECIFIED. ) 
 CURVE ( )  GEOMETRIC_REPRESENTATION_ITEM ( )  RATIONAL_B_SPLINE_CURVE ( ( 0.9999999999999995559, 0.8660254037844391517, 1.000000000000000000, 0.8660254037844387076, 1.000000000000000000, 0.8660254037844387076, 1.000000000000000000 ) ) 
 REPRESENTATION_ITEM ( '' )  );
#6341 = DIRECTION ( 'NONE',  ( 0.000000000000000000, -0.8660254037844387076, -0.5000000000000001110 ) ) ;
#6342 = EDGE_CURVE ( 'NONE', #10466, #8102, #9181, .T. ) ;
#6343 = FACE_BOUND ( 'NONE', #8434, .T. ) ;
#6344 = LINE ( 'NONE', #1309, #9359 ) ;
#6345 = AXIS2_PLACEMENT_3D ( 'NONE', #1217, #10247, #9199 ) ;
#6346 = DIRECTION ( 'NONE',  ( 0.000000000000000000, -1.000000000000000000, 0.000000000000000000 ) ) ;
#6347 = ORIENTED_EDGE ( 'NONE', *, *, #11898, .T. ) ;
#6348 = PRODUCT_DEFINITION_FORMATION_WITH_SPECIFIED_SOURCE ( 'ANY', '', #8352, .NOT_KNOWN. ) ;
#6349 = CARTESIAN_POINT ( 'NONE',  ( 35.00000000000000711, 53.69209320379640360, 4.071875000614516793 ) ) ;
#6350 = ORIENTED_EDGE ( 'NONE', *, *, #4091, .F. ) ;
#6351 = CARTESIAN_POINT ( 'NONE',  ( 20.00000000000000355, 0.000000000000000000, 1.500000000000000444 ) ) ;
#6352 = ORIENTED_EDGE ( 'NONE', *, *, #1216, .F. ) ;
#6353 = VECTOR ( 'NONE', #8082, 1000.000000000000000 ) ;
#6354 = CARTESIAN_POINT ( 'NONE',  ( 19.27821517812500574, 117.2309300971526937, 4.334375000614516971 ) ) ;
#6355 = PRODUCT_DEFINITION_SHAPE ( 'NONE', 'NONE',  #12256 ) ;
#6356 = ORIENTED_EDGE ( 'NONE', *, *, #300, .T. ) ;
#6357 = EDGE_CURVE ( 'NONE', #10050, #8873, #204, .T. ) ;
#6358 = VECTOR ( 'NONE', #4492, 1000.000000000000000 ) ;
#6359 = DIRECTION ( 'NONE',  ( 0.000000000000000000, 0.000000000000000000, 1.000000000000000000 ) ) ;
#6360 = CARTESIAN_POINT ( 'NONE',  ( 43.71630314554308683, 62.34089554097972297, 1.000000000000003109 ) ) ;
#6361 = EDGE_CURVE ( 'NONE', #6389, #8114, #12933, .T. ) ;
#6362 = CARTESIAN_POINT ( 'NONE',  ( 66.44356964374999563, 90.00000000000000000, 3.734375000614516882 ) ) ;
#6363 = CYLINDRICAL_SURFACE ( 'NONE', #5595, 6.499999999999999112 ) ;
#6364 = CARTESIAN_POINT ( 'NONE',  ( 1.000000000000000000, -5.473461295629626022, -0.8000000000000000444 ) ) ;
#6365 = CARTESIAN_POINT ( 'NONE',  ( 1.749999999999999112, 0.000000000000000000, 0.000000000000000000 ) ) ;
#6366 = AXIS2_PLACEMENT_3D ( 'NONE', #9889, #5776, #8786 ) ;
#6367 = CARTESIAN_POINT ( 'NONE',  ( 0.1325741768533960085, -4.273461295629625845, -0.8000000000000000444 ) ) ;
#6368 = DIRECTION ( 'NONE',  ( 1.000000000000000000, -0.000000000000000000, -0.000000000000000000 ) ) ;
#6369 = PLANE ( 'NONE',  #10539 ) ;
#6370 = DIRECTION ( 'NONE',  ( 0.000000000000000000, 0.000000000000000000, 1.000000000000000000 ) ) ;
#6371 = EDGE_CURVE ( 'NONE', #1472, #9206, #5258, .T. ) ;
#6372 = CARTESIAN_POINT ( 'NONE',  ( 1.040000000000000036, 0.000000000000000000, 0.000000000000000000 ) ) ;
#6373 = AXIS2_PLACEMENT_3D ( 'NONE', #12477, #5728, #4692 ) ;
#6374 = FACE_OUTER_BOUND ( 'NONE', #1119, .T. ) ;
#6375 = VERTEX_POINT ( 'NONE', #2326 ) ;
#6376 = VECTOR ( 'NONE', #3683, 1000.000000000000000 ) ;
#6377 = DIRECTION ( 'NONE',  ( 1.049727191973305394E-16, 0.5150380737757255245, -0.8571673013836856869 ) ) ;
#6378 = ORIENTED_EDGE ( 'NONE', *, *, #1729, .T. ) ;
#6379 = EDGE_CURVE ( 'NONE', #6201, #12851, #398, .T. ) ;
#6380 = LINE ( 'NONE', #1281, #7695 ) ;
#6381 = LINE ( 'NONE', #8355, #4304 ) ;
#6382 = CONICAL_SURFACE ( 'NONE', #11401, 1.499999999999999556, 1.029744259999998190 ) ;
#6383 = CARTESIAN_POINT ( 'NONE',  ( -60.00000000000000000, 30.00000000000000000, -10.00000000000000355 ) ) ;
#6384 = ORIENTED_EDGE ( 'NONE', *, *, #10311, .T. ) ;
#6385 = DIRECTION ( 'NONE',  ( 0.000000000000000000, 0.000000000000000000, -1.000000000000000000 ) ) ;
#6386 = CARTESIAN_POINT ( 'NONE',  ( 35.00000000000000000, 126.3079067962036106, 4.690625000614517148 ) ) ;
#6387 = ORIENTED_EDGE ( 'NONE', *, *, #12882, .T. ) ;
#6388 = FILL_AREA_STYLE_COLOUR ( '', #3434 ) ;
#6389 = VERTEX_POINT ( 'NONE', #8534 ) ;
#6390 = ORIENTED_EDGE ( 'NONE', *, *, #1049, .T. ) ;
#6391 = VECTOR ( 'NONE', #9273, 1000.000000000000000 ) ;
#6392 = CARTESIAN_POINT ( 'NONE',  ( 3.800000000000015365, 90.00000000000000000, 4.662500001229034297 ) ) ;
#6393 = LINE ( 'NONE', #4572, #1426 ) ;
#6394 = ORIENTED_EDGE ( 'NONE', *, *, #12712, .T. ) ;
#6395 = ADVANCED_FACE ( 'NONE', ( #5445 ), #2577, .T. ) ;
#6396 = ADVANCED_FACE ( 'NONE', ( #7544 ), #11402, .T. ) ;
#6397 = ORIENTED_EDGE ( 'NONE', *, *, #10309, .T. ) ;
#6398 = DIRECTION ( 'NONE',  ( -0.000000000000000000, 0.000000000000000000, 1.000000000000000000 ) ) ;
#6399 = ORIENTED_EDGE ( 'NONE', *, *, #3616, .T. ) ;
#6400 = CARTESIAN_POINT ( 'NONE',  ( 53.66639336120024950, 115.0996716663835571, 3.000000000000001776 ) ) ;
#6401 = ITEM_DEFINED_TRANSFORMATION ( 'NONE', 'NONE', #10731,  #5704 ) ;
#6402 = CARTESIAN_POINT ( 'NONE',  ( 3.800000000000015365, 90.00000000000000000, 3.762500001229034385 ) ) ;
#6403 = AXIS2_PLACEMENT_3D ( 'NONE', #12271, #8086, #12204 ) ;
#6404 = VERTEX_POINT ( 'NONE', #9375 ) ;
#6405 = DIRECTION ( 'NONE',  ( 1.000000000000000000, -0.000000000000000000, 0.000000000000000000 ) ) ;
#6406 = ORIENTED_EDGE ( 'NONE', *, *, #2964, .F. ) ;
#6407 = PLANE ( 'NONE',  #1491 ) ;
#6408 = VERTEX_POINT ( 'NONE', #7480 ) ;
#6409 = CARTESIAN_POINT ( 'NONE',  ( -1.000000000000000000, -4.873461295629625489, 0.000000000000000000 ) ) ;
#6410 = DIRECTION ( 'NONE',  ( 1.000000000000000000, 0.000000000000000000, -0.000000000000000000 ) ) ;
#6411 = VECTOR ( 'NONE', #9760, 1000.000000000000000 ) ;
#6412 = ORIENTED_EDGE ( 'NONE', *, *, #1030, .T. ) ;
#6413 = CARTESIAN_POINT ( 'NONE',  ( 3.800000000000015365, 90.00000000000000000, 4.212500001229034119 ) ) ;
#6414 = ORIENTED_EDGE ( 'NONE', *, *, #3723, .T. ) ;
#6415 = ADVANCED_FACE ( 'NONE', ( #4606 ), #9507, .F. ) ;
#6416 = LINE ( 'NONE', #654, #5215 ) ;
#6417 = CARTESIAN_POINT ( 'NONE',  ( 50.72178482187501203, 62.76906990284730625, 3.659375000614517592 ) ) ;
#6418 = ORIENTED_EDGE ( 'NONE', *, *, #4062, .T. ) ;
#6419 = AXIS2_PLACEMENT_3D ( 'NONE', #9258, #8284, #3321 ) ;
#6420 = DIRECTION ( 'NONE',  ( -0.000000000000000000, -0.000000000000000000, -1.000000000000000000 ) ) ;
#6421 = CARTESIAN_POINT ( 'NONE',  ( 10.74370178410656962, 110.0340209993050706, 3.000000000000000888 ) ) ;
#6422 = CARTESIAN_POINT ( 'NONE',  ( 50.72178482187499071, 117.2309300971526937, 4.259375000614517681 ) ) ;
#6423 = DIRECTION ( 'NONE',  ( -0.000000000000000000, 1.000000000000000000, -0.000000000000000000 ) ) ;
#6424 = LINE ( 'NONE', #5379, #12725 ) ;
#6425 = ADVANCED_FACE ( 'NONE', ( #1592 ), #8467, .F. ) ;
#6426 = DIRECTION ( 'NONE',  ( 0.3090169943749451753, 0.9510565162951544194, -0.000000000000000000 ) ) ;
#6427 = EDGE_CURVE ( 'NONE', #4076, #6279, #6556, .T. ) ;
#6428 = VECTOR ( 'NONE', #10359, 1000.000000000000000 ) ;
#6429 = DIRECTION ( 'NONE',  ( 1.000000000000000000, 0.000000000000000000, 0.000000000000000000 ) ) ;
#6430 = EDGE_CURVE ( 'NONE', #8420, #427, #6424, .T. ) ;
#6431 = CARTESIAN_POINT ( 'NONE',  ( 31.65768047819777919, 88.96129878493390208, 6.000000000000000000 ) ) ;
#6432 = DIRECTION ( 'NONE',  ( -0.000000000000000000, 1.000000000000000000, 0.000000000000000000 ) ) ;
#6433 = LINE ( 'NONE', #1599, #4921 ) ;
#6434 = CARTESIAN_POINT ( 'NONE',  ( -48.33333333333332860, 0.000000000000000000, -1.734723475976807094E-15 ) ) ;
#6435 = CARTESIAN_POINT ( 'NONE',  ( 45.00000000000000000, 0.000000000000000000, 7.250000000000001776 ) ) ;
#6436 = ORIENTED_EDGE ( 'NONE', *, *, #9753, .T. ) ;
#6437 = CIRCLE ( 'NONE', #10207, 1.000000000000000000 ) ;
#6438 = LINE ( 'NONE', #10435, #231 ) ;
#6439 = FACE_BOUND ( 'NONE', #4337, .T. ) ;
#6440 = ORIENTED_EDGE ( 'NONE', *, *, #9934, .T. ) ;
#6441 =( NAMED_UNIT ( * ) SI_UNIT ( $, .STERADIAN. ) SOLID_ANGLE_UNIT ( ) );
#6442 = ADVANCED_FACE ( 'NONE', ( #2516 ), #12521, .T. ) ;
#6443 = LINE ( 'NONE', #11616, #914 ) ;
#6444 = CARTESIAN_POINT ( 'NONE',  ( 66.19999999999998863, 90.00000000000000000, 4.774999999999999467 ) ) ;
#6445 = CARTESIAN_POINT ( 'NONE',  ( 1.269999999999999796, 0.000000000000000000, 0.000000000000000000 ) ) ;
#6446 = AXIS2_PLACEMENT_3D ( 'NONE', #9416, #8382, #8183 ) ;
#6447 = ORIENTED_EDGE ( 'NONE', *, *, #9012, .T. ) ;
#6448 = DIRECTION ( 'NONE',  ( 0.4444274669107966536, -0.8958148394926558344, 2.622474642788943734E-17 ) ) ;
#6449 = FACE_OUTER_BOUND ( 'NONE', #3648, .T. ) ;
#6450 = ORIENTED_EDGE ( 'NONE', *, *, #5037, .T. ) ;
#6451 = DIRECTION ( 'NONE',  ( 1.000000000000000000, 0.000000000000000000, 0.000000000000000000 ) ) ;
#6452 = VERTEX_POINT ( 'NONE', #10423 ) ;
#6453 = CIRCLE ( 'NONE', #8373, 1.499999999999998668 ) ;
#6454 = CARTESIAN_POINT ( 'NONE',  ( 33.50000000000000711, 67.79999999999999716, 6.000000000000000000 ) ) ;
#6455 = EDGE_LOOP ( 'NONE', ( #5848, #3295, #4191, #4649 ) ) ;
#6456 = CIRCLE ( 'NONE', #1665, 4.999999999999997335 ) ;
#6457 = CARTESIAN_POINT ( 'NONE',  ( 19.40000000000002700, 62.98000740192551206, 3.837500001229034563 ) ) ;
#6458 = CARTESIAN_POINT ( 'NONE',  ( 35.00000000000000000, 90.00000000000000000, -3.799999999999999822 ) ) ;
#6459 = VERTEX_POINT ( 'NONE', #9439 ) ;
#6460 = EDGE_CURVE ( 'NONE', #6204, #2762, #4471, .T. ) ;
#6461 = PRODUCT_DEFINITION_SHAPE ( 'NONE', 'NONE',  #5290 ) ;
#6462 = ORIENTED_EDGE ( 'NONE', *, *, #3040, .T. ) ;
#6464 = LINE ( 'NONE', #9547, #1573 ) ;
#6463 = VECTOR ( 'NONE', #9687, 1000.000000000000000 ) ;
#6465 = VERTEX_POINT ( 'NONE', #3564 ) ;
#6466 = DIRECTION ( 'NONE',  ( -0.000000000000000000, 1.000000000000000000, -0.000000000000000000 ) ) ;
#6467 = CONTEXT_DEPENDENT_SHAPE_REPRESENTATION ( #3606, #3771 ) ;
#6468 = CARTESIAN_POINT ( 'NONE',  ( 3.800000000000015365, 108.0133283987163111, 3.275000001229034119 ) ) ;
#6469 = ORIENTED_EDGE ( 'NONE', *, *, #3442, .F. ) ;
#6470 =( NAMED_UNIT ( * ) PLANE_ANGLE_UNIT ( ) SI_UNIT ( $, .RADIAN. ) );
#6471 = ADVANCED_FACE ( 'NONE', ( #8315 ), #1175, .F. ) ;
#6472 = ORIENTED_EDGE ( 'NONE', *, *, #4228, .F. ) ;
#6473 = ADVANCED_FACE ( 'NONE', ( #7263 ), #10205, .F. ) ;
#6474 = DIRECTION ( 'NONE',  ( -0.8660254037844365982, -0.5000000000000036637, 0.000000000000000000 ) ) ;
#6475 = EDGE_LOOP ( 'NONE', ( #12155, #4516, #110, #3983, #11644, #12937, #8216, #6324, #9498, #881, #5945, #1921, #6058, #7474, #3705, #9275, #11575, #5424, #12476, #1237, #7654, #9259, #433, #1086, #6256 ) ) ;
#6476 = CARTESIAN_POINT ( 'NONE',  ( 35.75000000000000711, 93.26496554346289258, 4.800000000000000711 ) ) ;
#6477 = VECTOR ( 'NONE', #6061, 1000.000000000000000 ) ;
#6478 = FACE_OUTER_BOUND ( 'NONE', #1972, .T. ) ;
#6479 = UNCERTAINTY_MEASURE_WITH_UNIT (LENGTH_MEASURE( 1.000000000000000082E-05 ), #3190, 'distance_accuracy_value', 'NONE');
#6480 = ORIENTED_EDGE ( 'NONE', *, *, #1654, .T. ) ;
#6481 = CARTESIAN_POINT ( 'NONE',  ( 66.44356964374999563, 90.00000000000000000, 4.184375000614516615 ) ) ;
#6482 = ORIENTED_EDGE ( 'NONE', *, *, #7115, .F. ) ;
#6483 = LINE ( 'NONE', #7404, #6041 ) ;
#6484 = ORIENTED_EDGE ( 'NONE', *, *, #6326, .T. ) ;
#6485 = VECTOR ( 'NONE', #685, 1000.000000000000114 ) ;
#6486 = CARTESIAN_POINT ( 'NONE',  ( 8.499999999999998224, 71.85789451624832225, 1.000000000000000000 ) ) ;
#6487 = ORIENTED_EDGE ( 'NONE', *, *, #11483, .F. ) ;
#6488 = CARTESIAN_POINT ( 'NONE',  ( 3.799999999999985612, 108.0133283987162827, 4.062500000000000000 ) ) ;
#6489 = DIRECTION ( 'NONE',  ( -0.000000000000000000, -0.4999999999999999445, -0.8660254037844387076 ) ) ;
#6490 = CARTESIAN_POINT ( 'NONE',  ( 19.27821517812500574, 117.2309300971526937, 2.984375000614517326 ) ) ;
#6491 = CARTESIAN_POINT ( 'NONE',  ( 35.00000000000000711, 53.69209320379640360, 4.465625000614517504 ) ) ;
#6492 = EDGE_CURVE ( 'NONE', #1613, #5624, #11377, .T. ) ;
#6493 = DIRECTION ( 'NONE',  ( 0.000000000000000000, -1.000000000000000000, 0.000000000000000000 ) ) ;
#6494 = CARTESIAN_POINT ( 'NONE',  ( -60.00000000000000000, 30.00000000000000000, 2.500000000000000000 ) ) ;
#6495 = CARTESIAN_POINT ( 'NONE',  ( 9.999999999999994671, 76.58915998087155685, -2.500000000000000000 ) ) ;
#6496 = CARTESIAN_POINT ( 'NONE',  ( 7.266925296109192800, 98.48530998897412303, -1.000000000000000000 ) ) ;
#6497 = LINE ( 'NONE', #11536, #7405 ) ;
#6498 = CARTESIAN_POINT ( 'NONE',  ( 3.000000000000004441, 30.00000000000000000, -2.500000000000000000 ) ) ;
#6499 = AXIS2_PLACEMENT_3D ( 'NONE', #5425, #2306, #8385 ) ;
#6500 = DIRECTION ( 'NONE',  ( -1.000000000000000000, 0.000000000000000000, 0.000000000000000000 ) ) ;
#6501 = CARTESIAN_POINT ( 'NONE',  ( -16.33333333333332504, 30.00000000000000000, -7.999999999999996447 ) ) ;
#6502 = ORIENTED_EDGE ( 'NONE', *, *, #7427, .T. ) ;
#6503 = LINE ( 'NONE', #4422, #10485 ) ;
#6504 = DIRECTION ( 'NONE',  ( -0.000000000000000000, 1.000000000000000000, -0.000000000000000000 ) ) ;
#6505 = ORIENTED_EDGE ( 'NONE', *, *, #7629, .T. ) ;
#6506 = ADVANCED_FACE ( 'NONE', ( #12366 ), #4196, .F. ) ;
#6507 = MECHANICAL_DESIGN_GEOMETRIC_PRESENTATION_REPRESENTATION (  '', ( #12157 ), #11731 ) ;
#6508 = DIRECTION ( 'NONE',  ( -0.000000000000000000, -0.000000000000000000, -1.000000000000000000 ) ) ;
#6509 = LINE ( 'NONE', #10504, #12456 ) ;
#6510 = CARTESIAN_POINT ( 'NONE',  ( -48.33333333333332860, 2.000000000000001332, -1.734723475976807094E-15 ) ) ;
#6511 = ORIENTED_EDGE ( 'NONE', *, *, #10803, .T. ) ;
#6512 = CARTESIAN_POINT ( 'NONE',  ( 31.99902028769960438, 88.51116798584881451, -3.800000000000000266 ) ) ;
#6513 = DIRECTION ( 'NONE',  ( 1.000000000000000000, 0.000000000000000000, 0.000000000000000000 ) ) ;
#6514 = EDGE_LOOP ( 'NONE', ( #7462, #11770, #2046, #9962 ) ) ;
#6515 = DIRECTION ( 'NONE',  ( 0.000000000000000000, 0.000000000000000000, 1.000000000000000000 ) ) ;
#6516 = PLANE ( 'NONE',  #11824 ) ;
#6517 = VERTEX_POINT ( 'NONE', #12300 ) ;
#6518 = ADVANCED_FACE ( 'NONE', ( #11312 ), #377, .F. ) ;
#6519 = AXIS2_PLACEMENT_3D ( 'NONE', #2108, #6940, #7072 ) ;
#6520 = CARTESIAN_POINT ( 'NONE',  ( 19.40000000000000924, 117.0199925980744666, 4.474999999999999645 ) ) ;
#6521 = ORIENTED_EDGE ( 'NONE', *, *, #7923, .T. ) ;
#6522 = EDGE_CURVE ( 'NONE', #5066, #10861, #8249, .T. ) ;
#6523 = DIRECTION ( 'NONE',  ( 8.673617379884034486E-16, 5.007715329123921945E-16, 1.000000000000000000 ) ) ;
#6524 = CARTESIAN_POINT ( 'NONE',  ( 40.00000000000000000, 0.000000000000000000, 10.00000000000000000 ) ) ;
#6525 = ORIENTED_EDGE ( 'NONE', *, *, #2882, .T. ) ;
#6526 = DIRECTION ( 'NONE',  ( 1.000000000000000000, 0.000000000000000000, 5.337610695313252124E-17 ) ) ;
#6527 = ORIENTED_EDGE ( 'NONE', *, *, #3532, .T. ) ;
#6528 = AXIS2_PLACEMENT_3D ( 'NONE', #2820, #11771, #5938 ) ;
#6529 = DIRECTION ( 'NONE',  ( 1.000000000000000000, 0.000000000000000000, 0.000000000000000000 ) ) ;
#6530 = ORIENTED_EDGE ( 'NONE', *, *, #2837, .T. ) ;
#6531 = DIRECTION ( 'NONE',  ( 0.000000000000000000, 0.000000000000000000, 1.000000000000000000 ) ) ;
#6532 = ITEM_DEFINED_TRANSFORMATION ( 'NONE', 'NONE', #4690,  #5704 ) ;
#6533 = CARTESIAN_POINT ( 'NONE',  ( 3.800000000000025135, 71.98667160128366049, 3.350000001229034297 ) ) ;
#6534 = ORIENTED_EDGE ( 'NONE', *, *, #7294, .T. ) ;
#6535 = ORIENTED_EDGE ( 'NONE', *, *, #7511, .T. ) ;
#6536 = EDGE_CURVE ( 'NONE', #5937, #12562, #5398, .T. ) ;
#6537 = DIRECTION ( 'NONE',  ( 0.000000000000000000, 1.000000000000000000, 0.000000000000000000 ) ) ;
#6538 = VERTEX_POINT ( 'NONE', #12238 ) ;
#6539 = CARTESIAN_POINT ( 'NONE',  ( 22.35108503858844031, 61.36708817440415942, 3.000000000000000888 ) ) ;
#6540 = CARTESIAN_POINT ( 'NONE',  ( 35.75000000000000711, 93.50000000000000000, -3.000000000000000000 ) ) ;
#6541 = CIRCLE ( 'NONE', #9050, 1.499999999999999778 ) ;
#6543 = EDGE_CURVE ( 'NONE', #1209, #8873, #2165, .T. ) ;
#6542 = EDGE_LOOP ( 'NONE', ( #4849, #710, #8452, #1097 ) ) ;
#6544 = CARTESIAN_POINT ( 'NONE',  ( 66.44356964374999563, 71.84604660189820891, 3.246875000614517059 ) ) ;
#6545 = ORIENTED_EDGE ( 'NONE', *, *, #1625, .T. ) ;
#6546 = LINE ( 'NONE', #5570, #3966 ) ;
#6547 = MECHANICAL_DESIGN_GEOMETRIC_PRESENTATION_REPRESENTATION (  '', ( #1959 ), #3423 ) ;
#6548 = VERTEX_POINT ( 'NONE', #12171 ) ;
#6549 = CARTESIAN_POINT ( 'NONE',  ( 3.556430356250028790, 71.84604660189818048, 3.096875000614517592 ) ) ;
#6550 = ORIENTED_EDGE ( 'NONE', *, *, #2837, .F. ) ;
#6551 = LINE ( 'NONE', #727, #7754 ) ;
#6552 = CLOSED_SHELL ( 'NONE', ( #11674, #8030, #11398, #8916, #12572, #1112, #4559, #5099, #12746, #9252, #11872, #5602, #3890, #3403, #5016, #9315, #2664, #8843, #1395, #6797, #12499, #2966, #335, #3814, #221, #7883, #8738, #900, #607, #6212, #12571, #9144, #9590, #3597, #11005, #260, #12092, #8433, #2323, #5322, #10347, #9826, #7155, #7820, #11907, #579, #3508 ) ) ;
#6553 = CARTESIAN_POINT ( 'NONE',  ( 3.640153284139971746, 92.50862168353172876, 3.000000000000000000 ) ) ;
#6554 = CARTESIAN_POINT ( 'NONE',  ( -6.666666666666660745, 2.000000000000000000, 0.000000000000000000 ) ) ;
#6555 = DIRECTION ( 'NONE',  ( 0.000000000000000000, 0.000000000000000000, 1.000000000000000000 ) ) ;
#6556 = LINE ( 'NONE', #532, #2290 ) ;
#6557 = PRODUCT_DEFINITION_FORMATION_WITH_SPECIFIED_SOURCE ( 'ANY', '', #5313, .NOT_KNOWN. ) ;
#6558 = DIRECTION ( 'NONE',  ( -0.8660254037844393737, -0.4999999999999987232, 0.000000000000000000 ) ) ;
#6559 = ADVANCED_FACE ( 'NONE', ( #12104 ), #5826, .F. ) ;
#6560 = DIRECTION ( 'NONE',  ( -0.000000000000000000, -0.000000000000000000, -1.000000000000000000 ) ) ;
#6561 = CARTESIAN_POINT ( 'NONE',  ( 31.80092274341787828, 89.00581455129388075, 4.800000000000000711 ) ) ;
#6562 = CYLINDRICAL_SURFACE ( 'NONE', #8861, 1.500000000000001332 ) ;
#6563 = VECTOR ( 'NONE', #9589, 1000.000000000000000 ) ;
#6564 = CARTESIAN_POINT ( 'NONE',  ( 38.50000000000000000, 90.00000000000000000, 22.38477631085024555 ) ) ;
#6565 = DIRECTION ( 'NONE',  ( 0.000000000000000000, 0.000000000000000000, 1.000000000000000000 ) ) ;
#6566 = CARTESIAN_POINT ( 'NONE',  ( 66.19999999999998863, 90.00000000000000000, 3.537500001229034297 ) ) ;
#6567 = ORIENTED_EDGE ( 'NONE', *, *, #8645, .F. ) ;
#6568 = LINE ( 'NONE', #477, #3717 ) ;
#6569 = ORIENTED_EDGE ( 'NONE', *, *, #6342, .F. ) ;
#6570 = CIRCLE ( 'NONE', #5740, 4.999999999999997335 ) ;
#6571 = AXIS2_PLACEMENT_3D ( 'NONE', #2441, #2373, #9363 ) ;
#6572 = FACE_OUTER_BOUND ( 'NONE', #834, .T. ) ;
#6573 = LINE ( 'NONE', #4624, #3225 ) ;
#6574 = ORIENTED_EDGE ( 'NONE', *, *, #8588, .T. ) ;
#6575 = VECTOR ( 'NONE', #1543, 1000.000000000000000 ) ;
#6576 = DIRECTION ( 'NONE',  ( 0.8958148394926558344, 0.4444274669107966536, 4.977592430910269431E-17 ) ) ;
#6577 = EDGE_CURVE ( 'NONE', #7985, #5120, #8748, .T. ) ;
#6578 = DIRECTION ( 'NONE',  ( -0.000000000000000000, -0.000000000000000000, -1.000000000000000000 ) ) ;
#6579 = AXIS2_PLACEMENT_3D ( 'NONE', #4720, #6735, #4908 ) ;
#6580 = ORIENTED_EDGE ( 'NONE', *, *, #12762, .F. ) ;
#6581 = CARTESIAN_POINT ( 'NONE',  ( 7.650000000000000355, 1.665213485140613626E-16, -1.219500000000000028 ) ) ;
#6582 = FACE_OUTER_BOUND ( 'NONE', #8902, .T. ) ;
#6583 = EDGE_LOOP ( 'NONE', ( #11821, #7904 ) ) ;
#6584 = CARTESIAN_POINT ( 'NONE',  ( -48.33333333333332860, -5.000000000000000000, -1.500000000000003109 ) ) ;
#6585 = VERTEX_POINT ( 'NONE', #4388 ) ;
#6586 = CARTESIAN_POINT ( 'NONE',  ( 35.00000000000000000, 90.00000000000000000, -1.000000000000000888 ) ) ;
#6587 = CIRCLE ( 'NONE', #5957, 10.00000000000000178 ) ;
#6588 = VECTOR ( 'NONE', #5209, 1000.000000000000000 ) ;
#6589 = CARTESIAN_POINT ( 'NONE',  ( 50.59999999999999432, 117.0199925980744666, 4.400000000000000355 ) ) ;
#6590 = EDGE_CURVE ( 'NONE', #4892, #8770, #803, .T. ) ;
#6591 = ORIENTED_EDGE ( 'NONE', *, *, #3401, .F. ) ;
#6592 = CARTESIAN_POINT ( 'NONE',  ( 35.00000000000000000, 90.00000000000000000, -8.000000000000000000 ) ) ;
#6593 = ORIENTED_EDGE ( 'NONE', *, *, #2400, .F. ) ;
#6594 = CARTESIAN_POINT ( 'NONE',  ( 35.00000000000000000, 90.00000000000000000, -18.00000000000000355 ) ) ;
#6595 = EDGE_CURVE ( 'NONE', #10269, #571, #9222, .T. ) ;
#6596 = PRODUCT_CONTEXT ( 'NONE', #55, 'mechanical' ) ;
#6597 = CARTESIAN_POINT ( 'NONE',  ( 3.800000000000015365, 90.00000000000000000, 3.312500001229034652 ) ) ;
#6598 = EDGE_LOOP ( 'NONE', ( #3608, #45, #7380, #9141 ) ) ;
#6599 = CIRCLE ( 'NONE', #11617, 6.499999999999999112 ) ;
#6600 = ORIENTED_EDGE ( 'NONE', *, *, #3372, .T. ) ;
#6601 = CIRCLE ( 'NONE', #7856, 1.599999999999990319 ) ;
#6602 = SURFACE_STYLE_USAGE ( .BOTH. , #4453 ) ;
#6603 = ORIENTED_EDGE ( 'NONE', *, *, #4361, .T. ) ;
#6604 = CARTESIAN_POINT ( 'NONE',  ( 4.452487237934602327, 82.57917759402269553, 2.999999999999998668 ) ) ;
#6605 = FACE_OUTER_BOUND ( 'NONE', #8112, .T. ) ;
#6606 = UNCERTAINTY_MEASURE_WITH_UNIT (LENGTH_MEASURE( 1.000000000000000082E-05 ), #8219, 'distance_accuracy_value', 'NONE');
#6607 = EDGE_CURVE ( 'NONE', #10599, #6015, #314, .T. ) ;
#6608 = ORIENTED_EDGE ( 'NONE', *, *, #6993, .T. ) ;
#6609 = VECTOR ( 'NONE', #3428, 1000.000000000000000 ) ;
#6610 = CARTESIAN_POINT ( 'NONE',  ( 35.00000000000000711, 53.97334320256736362, 4.325000001229033941 ) ) ;
#6611 = ORIENTED_EDGE ( 'NONE', *, *, #9626, .F. ) ;
#6612 = FACE_OUTER_BOUND ( 'NONE', #12750, .T. ) ;
#6613 = ORIENTED_EDGE ( 'NONE', *, *, #12600, .F. ) ;
#6614 = CARTESIAN_POINT ( 'NONE',  ( 50.72178482187499071, 117.2309300971526937, 3.359375000614517326 ) ) ;
#6615 = ORIENTED_EDGE ( 'NONE', *, *, #8639, .F. ) ;
#6616 = CARTESIAN_POINT ( 'NONE',  ( -61.13397459621560159, 31.96410161513775350, 0.000000000000000000 ) ) ;
#6617 = CARTESIAN_POINT ( 'NONE',  ( 30.00000000000000711, 2.000000000000000000, 10.00000000000000000 ) ) ;
#6618 = VECTOR ( 'NONE', #1847, 1000.000000000000000 ) ;
#6619 = CYLINDRICAL_SURFACE ( 'NONE', #12371, 1.599999999999992539 ) ;
#6620 = DIRECTION ( 'NONE',  ( -1.000000000000000000, 0.000000000000000000, 0.000000000000000000 ) ) ;
#6621 = CARTESIAN_POINT ( 'NONE',  ( 7.500000000000000000, 27.00000000000000000, -1.599999999999986766 ) ) ;
#6622 = ADVANCED_FACE ( 'NONE', ( #7197 ), #10338, .F. ) ;
#6623 = DIRECTION ( 'NONE',  ( -0.000000000000000000, -1.000000000000000000, -0.000000000000000000 ) ) ;
#6624 = CARTESIAN_POINT ( 'NONE',  ( 67.70000000000001705, 90.00000000000000000, 6.000000000000000000 ) ) ;
#6625 = CARTESIAN_POINT ( 'NONE',  ( 0.000000000000000000, 0.4117131682837005258, 0.000000000000000000 ) ) ;
#6626 = AXIS2_PLACEMENT_3D ( 'NONE', #6184, #2397, #4233 ) ;
#6627 = DIRECTION ( 'NONE',  ( -0.000000000000000000, 1.000000000000000000, -0.000000000000000000 ) ) ;
#6628 = DIRECTION ( 'NONE',  ( -0.000000000000000000, -0.000000000000000000, -1.000000000000000000 ) ) ;
#6629 = FACE_OUTER_BOUND ( 'NONE', #3781, .T. ) ;
#6631 = EDGE_CURVE ( 'NONE', #9145, #2190, #11249, .T. ) ;
#6630 = EDGE_LOOP ( 'NONE', ( #10481, #10907, #9534, #8792 ) ) ;
#6632 = EDGE_CURVE ( 'NONE', #7517, #1497, #4262, .T. ) ;
#6633 = CARTESIAN_POINT ( 'NONE',  ( 50.59999999999999432, 117.0199925980744666, 3.950000000000000178 ) ) ;
#6634 = DIRECTION ( 'NONE',  ( -0.000000000000000000, -0.000000000000000000, -1.000000000000000000 ) ) ;
#6635 = VERTEX_POINT ( 'NONE', #10268 ) ;
#6636 = AXIS2_PLACEMENT_3D ( 'NONE', #5563, #9558, #6410 ) ;
#6637 = SHAPE_REPRESENTATION_RELATIONSHIP ( 'NONE' , 'NONE' ,  #2422, #7935 ) ;
#6638 = FACE_OUTER_BOUND ( 'NONE', #8711, .T. ) ;
#6639 = LINE ( 'NONE', #2665, #4467 ) ;
#6640 = ORIENTED_EDGE ( 'NONE', *, *, #2870, .T. ) ;
#6641 = DIRECTION ( 'NONE',  ( -0.000000000000000000, 0.5000000000000003331, 0.8660254037844384856 ) ) ;
#6642 = VECTOR ( 'NONE', #3061, 1000.000000000000000 ) ;
#6643 = CARTESIAN_POINT ( 'NONE',  ( 66.44356964374998142, 108.1539533981018053, 3.265625000614517326 ) ) ;
#6644 = AXIS2_PLACEMENT_3D ( 'NONE', #6927, #12029, #3142 ) ;
#6645 = CYLINDRICAL_SURFACE ( 'NONE', #11912, 6.499999999999999112 ) ;
#6646 = DIRECTION ( 'NONE',  ( 0.000000000000000000, 0.000000000000000000, -1.000000000000000000 ) ) ;
#6647 = ORIENTED_EDGE ( 'NONE', *, *, #6652, .F. ) ;
#6648 = CARTESIAN_POINT ( 'NONE',  ( 38.40477530926831662, 84.46307801270444315, 4.000000000000000000 ) ) ;
#6649 = VERTEX_POINT ( 'NONE', #9441 ) ;
#6650 = CARTESIAN_POINT ( 'NONE',  ( 45.00000000000000000, -5.000000000000000000, 5.750000000000000888 ) ) ;
#6651 = DIRECTION ( 'NONE',  ( -1.000000000000000000, -0.000000000000000000, -0.000000000000000000 ) ) ;
#6652 = EDGE_CURVE ( 'NONE', #619, #8267, #11533, .T. ) ;
#6653 = AXIS2_PLACEMENT_3D ( 'NONE', #11334, #1392, #8145 ) ;
#6654 = CARTESIAN_POINT ( 'NONE',  ( 9.999999999999994671, 70.41451884327426569, 2.500000000000000444 ) ) ;
#6655 = ORIENTED_EDGE ( 'NONE', *, *, #9679, .F. ) ;
#6656 = PLANE ( 'NONE',  #9510 ) ;
#6657 = ORIENTED_EDGE ( 'NONE', *, *, #5145, .T. ) ;
#6658 = CARTESIAN_POINT ( 'NONE',  ( 45.00000000000000000, 0.000000000000000000, 4.249999999999999112 ) ) ;
#6659 = CONTEXT_DEPENDENT_SHAPE_REPRESENTATION ( #7853, #92 ) ;
#6660 = LINE ( 'NONE', #702, #3772 ) ;
#6661 = ORIENTED_EDGE ( 'NONE', *, *, #10289, .F. ) ;
#6662 = AXIS2_PLACEMENT_3D ( 'NONE', #6948, #2844, #6027 ) ;
#6663 =( NAMED_UNIT ( * ) SI_UNIT ( $, .STERADIAN. ) SOLID_ANGLE_UNIT ( ) );
#6664 = VERTEX_POINT ( 'NONE', #11404 ) ;
#6665 = VECTOR ( 'NONE', #10560, 999.9999999999998863 ) ;
#6666 = EDGE_CURVE ( 'NONE', #12180, #1278, #1523, .T. ) ;
#6667 = DIRECTION ( 'NONE',  ( -0.000000000000000000, 1.000000000000000000, -0.000000000000000000 ) ) ;
#6668 = EDGE_LOOP ( 'NONE', ( #644, #2231, #6730, #12036 ) ) ;
#6669 = CARTESIAN_POINT ( 'NONE',  ( 12.43081896414492782, 68.21485176374228843, 3.000000000000000888 ) ) ;
#6670 = CARTESIAN_POINT ( 'NONE',  ( 3.800000000000015365, 90.00000000000000000, 3.200000000000000178 ) ) ;
#6671 = EDGE_CURVE ( 'NONE', #1989, #443, #11335, .T. ) ;
#6672 = VECTOR ( 'NONE', #452, 1000.000000000000000 ) ;
#6673 = ORIENTED_EDGE ( 'NONE', *, *, #8569, .T. ) ;
#6674 = CARTESIAN_POINT ( 'NONE',  ( 16.96438320935645905, 66.02675393316422969, -3.000000000000000000 ) ) ;
#6675 = EDGE_LOOP ( 'NONE', ( #2205, #1885, #6469, #5048 ) ) ;
#6676 = CARTESIAN_POINT ( 'NONE',  ( 62.73514746974691292, 98.48596457872595522, -1.000000000000000000 ) ) ;
#6677 = VERTEX_POINT ( 'NONE', #6621 ) ;
#6678 = CARTESIAN_POINT ( 'NONE',  ( 19.27821517812500574, 117.2309300971526937, 3.378125000614517148 ) ) ;
#6679 = ORIENTED_EDGE ( 'NONE', *, *, #1016, .F. ) ;
#6680 = AXIS2_PLACEMENT_3D ( 'NONE', #9269, #9335, #9397 ) ;
#6681 = LINE ( 'NONE', #786, #10473 ) ;
#6682 = DIRECTION ( 'NONE',  ( -0.000000000000000000, -0.000000000000000000, 1.000000000000000000 ) ) ;
#6683 = EDGE_CURVE ( 'NONE', #767, #9108, #2712, .T. ) ;
#6684 = FILL_AREA_STYLE_COLOUR ( '', #4656 ) ;
#6685 = CARTESIAN_POINT ( 'NONE',  ( 3.556430356250014579, 108.1539533981018053, 3.415625000614517237 ) ) ;
#6686 = DIRECTION ( 'NONE',  ( 0.000000000000000000, -0.5000000000000003331, -0.8660254037844384856 ) ) ;
#6687 = AXIS2_PLACEMENT_3D ( 'NONE', #5263, #9253, #276 ) ;
#6688 = CARTESIAN_POINT ( 'NONE',  ( 35.00000000000000000, 90.00000000000000000, 6.000000000000000000 ) ) ;
#6689 = VECTOR ( 'NONE', #8405, 1000.000000000000000 ) ;
#6690 = LINE ( 'NONE', #8723, #5833 ) ;
#6691 = LINE ( 'NONE', #859, #12435 ) ;
#6692 = CARTESIAN_POINT ( 'NONE',  ( 21.49999999999998579, 90.00000000000000000, -10.00000000000000000 ) ) ;
#6693 = CARTESIAN_POINT ( 'NONE',  ( 50.00000000000000000, 2.000000000000001776, -1.500000000000000000 ) ) ;
#6694 = CARTESIAN_POINT ( 'NONE',  ( 19.27821517812500574, 117.2309300971526937, 4.784375000614516260 ) ) ;
#6695 = VERTEX_POINT ( 'NONE', #8599 ) ;
#6696 = ADVANCED_FACE ( 'NONE', ( #10620, #7481 ), #4473, .F. ) ;
#6697 = CARTESIAN_POINT ( 'NONE',  ( 19.40000000000000924, 117.0199925980744666, 3.125000000000000000 ) ) ;
#6698 = CIRCLE ( 'NONE', #10248, 3.499999999999996003 ) ;
#6699 = CARTESIAN_POINT ( 'NONE',  ( -36.66666666666665009, 46.12451549659709116, -7.999999999999996447 ) ) ;
#6700 = ORIENTED_EDGE ( 'NONE', *, *, #11234, .T. ) ;
#6701 =( NAMED_UNIT ( * ) PLANE_ANGLE_UNIT ( ) SI_UNIT ( $, .RADIAN. ) );
#6702 = CARTESIAN_POINT ( 'NONE',  ( 35.75000000000000711, 93.41869858279433458, -3.000000000000000000 ) ) ;
#6703 = EDGE_CURVE ( 'NONE', #1821, #5315, #1594, .T. ) ;
#6704 = CARTESIAN_POINT ( 'NONE',  ( 45.39999948872177526, 60.58435772187547030, 2.999999999999999556 ) ) ;
#6705 = EDGE_CURVE ( 'NONE', #11236, #330, #4376, .T. ) ;
#6706=STYLED_ITEM('',(#13016),#11745);
#6707 = CARTESIAN_POINT ( 'NONE',  ( 40.00000000000000000, 2.000000000000000000, -10.00000000000000000 ) ) ;
#6708 = CYLINDRICAL_SURFACE ( 'NONE', #1248, 1.500000000000001332 ) ;
#6709 = CARTESIAN_POINT ( 'NONE',  ( 35.00000000000000000, 90.00000000000000000, 4.000000000000000000 ) ) ;
#6710 = CARTESIAN_POINT ( 'NONE',  ( 50.72178482187501203, 62.76906990284730625, 4.559375000614517504 ) ) ;
#6711 = VERTEX_POINT ( 'NONE', #8469 ) ;
#6712 = CARTESIAN_POINT ( 'NONE',  ( -38.66666666666665719, 30.00000000000000000, -7.999999999999996447 ) ) ;
#6713 = ORIENTED_EDGE ( 'NONE', *, *, #7105, .T. ) ;
#6714 = EDGE_CURVE ( 'NONE', #11446, #3791, #9509, .T. ) ;
#6715 = CARTESIAN_POINT ( 'NONE',  ( 0.000000000000000000, 0.000000000000000000, 0.000000000000000000 ) ) ;
#6716 = FACE_OUTER_BOUND ( 'NONE', #1535, .T. ) ;
#6717 = CARTESIAN_POINT ( 'NONE',  ( 66.19999999999998863, 90.00000000000000000, 3.987500001229034030 ) ) ;
#6718 = LINE ( 'NONE', #2806, #4675 ) ;
#6719 = EDGE_LOOP ( 'NONE', ( #1622, #1057 ) ) ;
#6720 = EDGE_CURVE ( 'NONE', #6465, #4984, #2386, .T. ) ;
#6721 = DIRECTION ( 'NONE',  ( 1.000000000000000000, 1.914177628664063178E-15, -0.000000000000000000 ) ) ;
#6722 = EDGE_LOOP ( 'NONE', ( #3545, #903, #3000, #8917 ) ) ;
#6723 = DIRECTION ( 'NONE',  ( -0.000000000000000000, 1.000000000000000000, -0.000000000000000000 ) ) ;
#6724 = CONTEXT_DEPENDENT_SHAPE_REPRESENTATION ( #12784, #2213 ) ;
#6725 = CARTESIAN_POINT ( 'NONE',  ( 35.00000000000000000, 90.00000000000000000, 1.000000000000000000 ) ) ;
#6726 = ORIENTED_EDGE ( 'NONE', *, *, #19, .F. ) ;
#6727 =( GEOMETRIC_REPRESENTATION_CONTEXT ( 3 ) GLOBAL_UNCERTAINTY_ASSIGNED_CONTEXT ( ( #3614 ) ) GLOBAL_UNIT_ASSIGNED_CONTEXT ( ( #2042, #7991, #2173 ) ) REPRESENTATION_CONTEXT ( 'NONE', 'WORKASPACE' ) );
#6728 = VERTEX_POINT ( 'NONE', #8535 ) ;
#6729 =( NAMED_UNIT ( * ) PLANE_ANGLE_UNIT ( ) SI_UNIT ( $, .RADIAN. ) );
#6730 = ORIENTED_EDGE ( 'NONE', *, *, #12241, .T. ) ;
#6731 = CARTESIAN_POINT ( 'NONE',  ( 42.32262610911597278, 59.65151212041654105, 2.999999999999999556 ) ) ;
#6732 = CARTESIAN_POINT ( 'NONE',  ( 3.800000000000015365, 90.00000000000000000, 5.000000000000000000 ) ) ;
#6733 = AXIS2_PLACEMENT_3D ( 'NONE', #5877, #10852, #6069 ) ;
#6734 = ORIENTED_EDGE ( 'NONE', *, *, #5956, .F. ) ;
#6735 = DIRECTION ( 'NONE',  ( 1.000000000000000000, 0.000000000000000000, -0.000000000000000000 ) ) ;
#6736 = EDGE_CURVE ( 'NONE', #8306, #8496, #12385, .T. ) ;
#6737 = EDGE_LOOP ( 'NONE', ( #12829, #6265, #7534, #8261 ) ) ;
#6738 = CARTESIAN_POINT ( 'NONE',  ( 25.00000000000000355, 2.000000000000001332, -4.150000000000012790 ) ) ;
#6739 = ORIENTED_EDGE ( 'NONE', *, *, #2003, .T. ) ;
#6740 = LINE ( 'NONE', #10733, #9885 ) ;
#6741 = EDGE_CURVE ( 'NONE', #7595, #1608, #1659, .T. ) ;
#6742 = ORIENTED_EDGE ( 'NONE', *, *, #747, .T. ) ;
#6743 = CARTESIAN_POINT ( 'NONE',  ( 30.00000000000000711, 0.000000000000000000, 10.00000000000000000 ) ) ;
#6744 = CARTESIAN_POINT ( 'NONE',  ( -0.9999999999999997780, -4.273461295629625845, 0.000000000000000000 ) ) ;
#6745 = CARTESIAN_POINT ( 'NONE',  ( -6.666666666666660745, 0.000000000000000000, 0.000000000000000000 ) ) ;
#6746 = CARTESIAN_POINT ( 'NONE',  ( 35.00000000000000711, 53.97334320256736362, 4.325000001229033941 ) ) ;
#6747 = AXIS2_PLACEMENT_3D ( 'NONE', #5232, #6081, #8248 ) ;
#6748 = DIRECTION ( 'NONE',  ( 0.000000000000000000, 0.000000000000000000, 1.000000000000000000 ) ) ;
#6749 = CYLINDRICAL_SURFACE ( 'NONE', #11612, 3.500000000000003109 ) ;
#6750 = COLOUR_RGB ( '',0.8941176470588234615, 0.8941176470588234615, 0.8941176470588234615 ) ;
#6751 = DIRECTION ( 'NONE',  ( -1.000000000000000000, 0.000000000000000000, 0.000000000000000000 ) ) ;
#6752 = EDGE_CURVE ( 'NONE', #7727, #977, #12457, .T. ) ;
#6753 = DIRECTION ( 'NONE',  ( -0.000000000000000000, -0.000000000000000000, -1.000000000000000000 ) ) ;
#6754 = LINE ( 'NONE', #12842, #9912 ) ;
#6755 = CLOSED_SHELL ( 'NONE', ( #9355, #12127, #3335, #3418, #7169, #11601, #9592, #9187, #6959, #2648, #12387, #12288, #5768, #6055, #351, #8162, #12671, #5815, #4757, #8288, #8794, #2769, #5377, #10301, #4999, #6696, #6892, #774, #10605, #2382, #3073, #12269, #4139, #12713, #7484, #6238, #11498, #5156 ) ) ;
#6756 = DIRECTION ( 'NONE',  ( -1.000000000000000000, -0.000000000000000000, -0.000000000000000000 ) ) ;
#6757 = EDGE_CURVE ( 'NONE', #488, #1106, #10008, .T. ) ;
#6758 =( REPRESENTATION_RELATIONSHIP ('NONE','NONE', #1997, #5582 ) REPRESENTATION_RELATIONSHIP_WITH_TRANSFORMATION ( #7648 )SHAPE_REPRESENTATION_RELATIONSHIP( ) );
#6759 = FACE_OUTER_BOUND ( 'NONE', #9777, .T. ) ;
#6760 = B_SPLINE_CURVE_WITH_KNOTS ( 'NONE', 3,
 ( #2776, #7999, #2967, #795 ),
 .UNSPECIFIED., .F., .F.,
 ( 4, 4 ),
 ( 0.000000000000000000, 1.000000000000000000 ),
 .UNSPECIFIED. ) ;
#6761 = CARTESIAN_POINT ( 'NONE',  ( 50.72178482187499071, 117.2309300971526937, 2.909375000614517148 ) ) ;
#6762 = VERTEX_POINT ( 'NONE', #3630 ) ;
#6764 = CARTESIAN_POINT ( 'NONE',  ( 66.20000000000000284, 71.98667160128370313, 3.837500000000000799 ) ) ;
#6763 = AXIS2_PLACEMENT_3D ( 'NONE', #5459, #4747, #8734 ) ;
#6765 = CARTESIAN_POINT ( 'NONE',  ( 66.19999999999998863, 90.00000000000000000, 3.537500001229034297 ) ) ;
#6766 = ORIENTED_EDGE ( 'NONE', *, *, #4289, .T. ) ;
#6767 =( NAMED_UNIT ( * ) PLANE_ANGLE_UNIT ( ) SI_UNIT ( $, .RADIAN. ) );
#6768 = AXIS2_PLACEMENT_3D ( 'NONE', #11091, #9332, #12214 ) ;
#6769 = VECTOR ( 'NONE', #8987, 1000.000000000000000 ) ;
#6770 = CARTESIAN_POINT ( 'NONE',  ( 0.000000000000000000, -1.154700538379251684, -1.199226976249124676E-17 ) ) ;
#6771 = EDGE_CURVE ( 'NONE', #4991, #12815, #6456, .T. ) ;
#6772 = DIRECTION ( 'NONE',  ( -1.000000000000000000, 0.000000000000000000, -0.000000000000000000 ) ) ;
#6773 = CARTESIAN_POINT ( 'NONE',  ( 12.66025403784434822, 85.80682368868758658, 1.000000000000000000 ) ) ;
#6774 = CARTESIAN_POINT ( 'NONE',  ( 3.556430356250015024, 90.00000000000000000, 3.903125000614517504 ) ) ;
#6775 = DIRECTION ( 'NONE',  ( -0.000000000000000000, 0.000000000000000000, -1.000000000000000000 ) ) ;
#6776 = CARTESIAN_POINT ( 'NONE',  ( 3.556430356250028790, 71.84604660189818048, 3.996875000614517504 ) ) ;
#6777 = ORIENTED_EDGE ( 'NONE', *, *, #10093, .T. ) ;
#6778 = CIRCLE ( 'NONE', #8674, 6.499999999999999112 ) ;
#6779 = FACE_BOUND ( 'NONE', #8683, .T. ) ;
#6780 = ORIENTED_EDGE ( 'NONE', *, *, #10388, .T. ) ;
#6781 = FACE_OUTER_BOUND ( 'NONE', #3732, .T. ) ;
#6782 = CARTESIAN_POINT ( 'NONE',  ( 35.00000000000000000, 90.00000000000000000, 3.000000000000000000 ) ) ;
#6783 = LINE ( 'NONE', #10779, #8015 ) ;
#6784 = CARTESIAN_POINT ( 'NONE',  ( -28.99038105676692112, 50.21281292110204930, -1.000000000000000000 ) ) ;
#6785 = AXIS2_PLACEMENT_3D ( 'NONE', #4319, #5550, #3406 ) ;
#6786 = DIRECTION ( 'NONE',  ( -1.000000000000000000, 0.000000000000000000, -0.000000000000000000 ) ) ;
#6787 = ORIENTED_EDGE ( 'NONE', *, *, #10990, .F. ) ;
#6788 = CARTESIAN_POINT ( 'NONE',  ( 0.1038759689922479496, -3.348389132562988646, 0.000000000000000000 ) ) ;
#6789 = DIRECTION ( 'NONE',  ( 0.9510565162951543083, -0.3090169943749451198, 0.000000000000000000 ) ) ;
#6790 = EDGE_LOOP ( 'NONE', ( #5594, #2674, #2739, #11064, #2910, #2103 ) ) ;
#6791 = CARTESIAN_POINT ( 'NONE',  ( -0.9999999999999997780, -4.273461295629625845, -0.8000000000000000444 ) ) ;
#6792 = VERTEX_POINT ( 'NONE', #399 ) ;
#6793 = CYLINDRICAL_SURFACE ( 'NONE', #4226, 31.19999999999999929 ) ;
#6795 = VERTEX_POINT ( 'NONE', #11467 ) ;
#6794 = AXIS2_PLACEMENT_3D ( 'NONE', #12808, #12878, #6980 ) ;
#6796 = EDGE_CURVE ( 'NONE', #8545, #6062, #2517, .T. ) ;
#6797 = ADVANCED_FACE ( 'NONE', ( #3435 ), #7416, .T. ) ;
#6798 = LINE ( 'NONE', #9013, #12379 ) ;
#6799 = CARTESIAN_POINT ( 'NONE',  ( -38.66666666666665719, 2.000000000000000000, 7.999999999999996447 ) ) ;
#6800 = ORIENTED_EDGE ( 'NONE', *, *, #1425, .F. ) ;
#6801 = LINE ( 'NONE', #11650, #86 ) ;
#6802 = ORIENTED_EDGE ( 'NONE', *, *, #5643, .T. ) ;
#6803 = AXIS2_PLACEMENT_3D ( 'NONE', #11339, #2391, #6370 ) ;
#6804 = DIRECTION ( 'NONE',  ( -0.000000000000000000, 1.000000000000000000, -0.000000000000000000 ) ) ;
#6805 = AXIS2_PLACEMENT_3D ( 'NONE', #6791, #4961, #2020 ) ;
#6806 = VERTEX_POINT ( 'NONE', #5447 ) ;
#6807 = CARTESIAN_POINT ( 'NONE',  ( 50.72178482187501203, 62.76906990284730625, 4.503125000614517148 ) ) ;
#6808 = ORIENTED_EDGE ( 'NONE', *, *, #7459, .F. ) ;
#6809 = CARTESIAN_POINT ( 'NONE',  ( 45.00000000000000000, 0.000000000000000000, 7.250000000000001776 ) ) ;
#6810 = CARTESIAN_POINT ( 'NONE',  ( 25.00000000000000355, 0.000000000000000000, -5.750000000000000000 ) ) ;
#6811 = CARTESIAN_POINT ( 'NONE',  ( 66.44356964374999563, 71.84604660189820891, 3.190625000614517592 ) ) ;
#6812 = AXIS2_PLACEMENT_3D ( 'NONE', #3590, #4631, #11557 ) ;
#6813 = FACE_OUTER_BOUND ( 'NONE', #7666, .T. ) ;
#6814 = ADVANCED_FACE ( 'NONE', ( #12522 ), #4734, .T. ) ;
#6815 = DIRECTION ( 'NONE',  ( 0.000000000000000000, 0.000000000000000000, 1.000000000000000000 ) ) ;
#6816 = DIRECTION ( 'NONE',  ( 0.000000000000000000, -1.000000000000000000, -0.000000000000000000 ) ) ;
#6817 = DIRECTION ( 'NONE',  ( -0.000000000000000000, -0.000000000000000000, -1.000000000000000000 ) ) ;
#6818 = DIRECTION ( 'NONE',  ( -0.000000000000000000, -1.000000000000000000, -0.000000000000000000 ) ) ;
#6819 = PLANE ( 'NONE',  #9528 ) ;
#6820 = ORIENTED_EDGE ( 'NONE', *, *, #500, .F. ) ;
#6821 = CONICAL_SURFACE ( 'NONE', #3498, 1.500000000000003331, 1.029744259999999967 ) ;
#6822 = DIRECTION ( 'NONE',  ( 0.000000000000000000, 0.000000000000000000, 1.000000000000000000 ) ) ;
#6823 = CARTESIAN_POINT ( 'NONE',  ( 66.44356964374998142, 108.1539533981018053, 3.321875000614517237 ) ) ;
#6824 = ORIENTED_EDGE ( 'NONE', *, *, #2826, .F. ) ;
#6825 = CARTESIAN_POINT ( 'NONE',  ( 19.40000000000002700, 62.98000740192551206, 3.725000000000000089 ) ) ;
#6826 = EDGE_CURVE ( 'NONE', #10249, #8545, #10808, .T. ) ;
#6827 = CARTESIAN_POINT ( 'NONE',  ( 31.72849223410691266, 88.75612020769642641, 4.000000000000000000 ) ) ;
#6828 = ORIENTED_EDGE ( 'NONE', *, *, #12589, .F. ) ;
#6829 = EDGE_CURVE ( 'NONE', #9537, #8099, #2963, .T. ) ;
#6830 = VECTOR ( 'NONE', #6377, 999.9999999999998863 ) ;
#6831 = CARTESIAN_POINT ( 'NONE',  ( 3.800000000000004707, 90.00000000000000000, 6.000000000000000000 ) ) ;
#6832 = DIRECTION ( 'NONE',  ( 0.000000000000000000, 0.000000000000000000, -1.000000000000000000 ) ) ;
#6833 = APPLICATION_CONTEXT ( 'automotive_design' ) ;
#6834 = CARTESIAN_POINT ( 'NONE',  ( -36.66666666666665009, 2.000000000000000000, -7.999999999999996447 ) ) ;
#6835 = CARTESIAN_POINT ( 'NONE',  ( 35.00000000000000000, 126.3079067962036106, 2.890625000614516882 ) ) ;
#6836 =( BOUNDED_CURVE ( )  B_SPLINE_CURVE ( 2, ( #12429, #4580, #3475, #7456, #3539, #11440, #9480 ),
 .UNSPECIFIED., .F., .F. ) 
 B_SPLINE_CURVE_WITH_KNOTS ( ( 3, 2, 2, 3 ),
 ( 0.000000000000000000, 0.03333333333333339532, 0.06666666666666679064, 0.1000000000000001860 ),
 .UNSPECIFIED. ) 
 CURVE ( )  GEOMETRIC_REPRESENTATION_ITEM ( )  RATIONAL_B_SPLINE_CURVE ( ( 1.000000000000000000, 0.8660254037844387076, 1.000000000000000000, 0.8660254037844387076, 1.000000000000000000, 0.8660254037844380415, 1.000000000000000666 ) ) 
 REPRESENTATION_ITEM ( '' )  );
#6837 = DIRECTION ( 'NONE',  ( -0.5877852522924753575, 0.8090169943749458970, 0.000000000000000000 ) ) ;
#6838 = DIRECTION ( 'NONE',  ( -0.000000000000000000, -0.000000000000000000, 1.000000000000000000 ) ) ;
#6839 = VERTEX_POINT ( 'NONE', #11726 ) ;
#6840 = VECTOR ( 'NONE', #10883, 1000.000000000000114 ) ;
#6841 = FACE_OUTER_BOUND ( 'NONE', #2303, .T. ) ;
#6842 = ORIENTED_EDGE ( 'NONE', *, *, #2054, .T. ) ;
#6843 = EDGE_CURVE ( 'NONE', #12533, #1608, #8719, .T. ) ;
#6844 =( NAMED_UNIT ( * ) SI_UNIT ( $, .STERADIAN. ) SOLID_ANGLE_UNIT ( ) );
#6845 = B_SPLINE_CURVE_WITH_KNOTS ( 'NONE', 3,
 ( #395, #6553, #528, #4407, #1519, #9504, #10288, #11397, #10357, #1321, #5575, #332, #8529, #6421, #4603, #8594, #4468 ),
 .UNSPECIFIED., .F., .F.,
 ( 4, 2, 1, 2, 2, 2, 2, 2, 4 ),
 ( 0.000000000000000000, 0.003052186405622107652, 0.006104372811244215304, 0.009156559216866321654, 0.01068265241967737700, 0.01220874562248843061, 0.01831311843373264331, 0.02136530483935476787, 0.02441749124497688897 ),
 .UNSPECIFIED. ) ;
#6846 = DIRECTION ( 'NONE',  ( -0.000000000000000000, 1.000000000000000000, -0.000000000000000000 ) ) ;
#6847 = LINE ( 'NONE', #5924, #3002 ) ;
#6848 = CIRCLE ( 'NONE', #3737, 1.000000000000000000 ) ;
#6849 = DIRECTION ( 'NONE',  ( 0.000000000000000000, 0.000000000000000000, 1.000000000000000000 ) ) ;
#6850 = AXIS2_PLACEMENT_3D ( 'NONE', #529, #1589, #8465 ) ;
#6851 = DIRECTION ( 'NONE',  ( 1.000000000000000000, 0.000000000000000000, 5.337610695313252124E-17 ) ) ;
#6852 = EDGE_LOOP ( 'NONE', ( #9820, #6608, #10510, #4846 ) ) ;
#6853 = DIRECTION ( 'NONE',  ( -1.000000000000000000, 0.000000000000000000, 0.000000000000000000 ) ) ;
#6854 = ITEM_DEFINED_TRANSFORMATION ( 'NONE', 'NONE', #5727,  #5704 ) ;
#6855 = DIRECTION ( 'NONE',  ( 0.8660254037844361541, 0.5000000000000042188, 0.000000000000000000 ) ) ;
#6856 = ORIENTED_EDGE ( 'NONE', *, *, #7250, .T. ) ;
#6857 = DIRECTION ( 'NONE',  ( -1.000000000000000000, 0.000000000000000000, -0.000000000000000000 ) ) ;
#6858 = ORIENTED_EDGE ( 'NONE', *, *, #5436, .F. ) ;
#6859 = ORIENTED_EDGE ( 'NONE', *, *, #2567, .F. ) ;
#6860 = ADVANCED_FACE ( 'NONE', ( #3886 ), #6944, .T. ) ;
#6861 = VECTOR ( 'NONE', #10664, 1000.000000000000000 ) ;
#6862 = DIRECTION ( 'NONE',  ( 0.4719909656437444867, -0.8816033849473842166, 0.000000000000000000 ) ) ;
#6863 = CARTESIAN_POINT ( 'NONE',  ( 50.60000000000001563, 62.98000740192552627, 3.350000000000000533 ) ) ;
#6864 = ORIENTED_EDGE ( 'NONE', *, *, #6194, .F. ) ;
#6865 = FACE_OUTER_BOUND ( 'NONE', #9873, .T. ) ;
#6866 = EDGE_LOOP ( 'NONE', ( #6233, #7189, #9486 ) ) ;
#6867 = ADVANCED_FACE ( 'NONE', ( #12903 ), #2502, .F. ) ;
#6868 = DIRECTION ( 'NONE',  ( -1.000000000000000000, 0.000000000000000000, 0.000000000000000000 ) ) ;
#6869 = CIRCLE ( 'NONE', #7288, 6.499999999999999112 ) ;
#6870 = ADVANCED_FACE ( 'NONE', ( #12714 ), #4669, .T. ) ;
#6871 = ORIENTED_EDGE ( 'NONE', *, *, #2856, .T. ) ;
#6872 = CARTESIAN_POINT ( 'NONE',  ( 19.27821517812500574, 117.2309300971526937, 2.928125000614517415 ) ) ;
#6873 = ORIENTED_EDGE ( 'NONE', *, *, #4599, .T. ) ;
#6874 = CARTESIAN_POINT ( 'NONE',  ( 62.73102604205943322, 98.48470356904833523, 3.000000000000000888 ) ) ;
#6875 = CARTESIAN_POINT ( 'NONE',  ( 66.19999999999998863, 90.00000000000000000, 3.875000000000000000 ) ) ;
#6876 = CARTESIAN_POINT ( 'NONE',  ( 66.19999999999998863, 90.00000000000000000, 3.537500001229034297 ) ) ;
#6877 = AXIS2_PLACEMENT_3D ( 'NONE', #12444, #4462, #1647 ) ;
#6878 = CARTESIAN_POINT ( 'NONE',  ( 19.40000000000002700, 62.98000740192551206, 4.287500001229034297 ) ) ;
#6879 = EDGE_CURVE ( 'NONE', #1672, #8022, #4171, .T. ) ;
#6880 = CIRCLE ( 'NONE', #1239, 1.219500000000000028 ) ;
#6881 = CARTESIAN_POINT ( 'NONE',  ( -67.46410161513773573, 36.92820323027551410, 2.500000000000000000 ) ) ;
#6882 = EDGE_LOOP ( 'NONE', ( #8395, #10715, #4003, #5332, #2159 ) ) ;
#6883 = PLANE ( 'NONE',  #1350 ) ;
#6884 = CARTESIAN_POINT ( 'NONE',  ( 35.00000000000000000, 90.00000000000000000, -3.000000000000000000 ) ) ;
#6885 = CARTESIAN_POINT ( 'NONE',  ( 1.649999999999999911, 0.000000000000000000, 0.000000000000000000 ) ) ;
#6886 = VERTEX_POINT ( 'NONE', #5958 ) ;
#6887 = VECTOR ( 'NONE', #4710, 1000.000000000000000 ) ;
#6888 = DIRECTION ( 'NONE',  ( 0.000000000000000000, 0.000000000000000000, 1.000000000000000000 ) ) ;
#6889 = ORIENTED_EDGE ( 'NONE', *, *, #678, .T. ) ;
#6890 = DIRECTION ( 'NONE',  ( -0.000000000000000000, 0.000000000000000000, -1.000000000000000000 ) ) ;
#6891 = CARTESIAN_POINT ( 'NONE',  ( 19.27821517812503060, 62.76906990284727783, 3.584375000614516971 ) ) ;
#6892 = ADVANCED_FACE ( 'NONE', ( #11918 ), #5774, .F. ) ;
#6893 = ORIENTED_EDGE ( 'NONE', *, *, #3837, .T. ) ;
#6894 = CARTESIAN_POINT ( 'NONE',  ( 19.27821517812503060, 62.76906990284727783, 4.034375000614517148 ) ) ;
#6895 = DIRECTION ( 'NONE',  ( 0.000000000000000000, 0.000000000000000000, 1.000000000000000000 ) ) ;
#6896 = VECTOR ( 'NONE', #4957, 1000.000000000000000 ) ;
#6897 = DIRECTION ( 'NONE',  ( -0.000000000000000000, -0.000000000000000000, 1.000000000000000000 ) ) ;
#6898 = CARTESIAN_POINT ( 'NONE',  ( 1.749999999999999112, 0.000000000000000000, 1.499999999999998668 ) ) ;
#6899 = ADVANCED_FACE ( 'NONE', ( #918 ), #2713, .T. ) ;
#6900 = CARTESIAN_POINT ( 'NONE',  ( 64.54728993811707483, 100.7543353701752125, 2.858851390224067313 ) ) ;
#6901 = CIRCLE ( 'NONE', #1896, 30.00000000000000000 ) ;
#6902 = CARTESIAN_POINT ( 'NONE',  ( 34.49999999999998579, 96.48074069840785683, -0.9999999999999970024 ) ) ;
#6903 = LINE ( 'NONE', #14, #12885 ) ;
#6904 = EDGE_CURVE ( 'NONE', #946, #1825, #10928, .T. ) ;
#6905 = ORIENTED_EDGE ( 'NONE', *, *, #11049, .T. ) ;
#6906 = PLANE ( 'NONE',  #2458 ) ;
#6907 = ORIENTED_EDGE ( 'NONE', *, *, #4213, .F. ) ;
#6908 = DIRECTION ( 'NONE',  ( 0.000000000000000000, 0.000000000000000000, 1.000000000000000000 ) ) ;
#6909 = AXIS2_PLACEMENT_3D ( 'NONE', #6616, #2642, #11460 ) ;
#6910 = DIRECTION ( 'NONE',  ( 0.000000000000000000, -0.8660254037844387076, 0.5000000000000001110 ) ) ;
#6911 = DIRECTION ( 'NONE',  ( 0.000000000000000000, 0.000000000000000000, 1.000000000000000000 ) ) ;
#6912 = CARTESIAN_POINT ( 'NONE',  ( -2.179634403564815859, -5.614030811971695734, -0.8000000000000000444 ) ) ;
#6913 =( BOUNDED_CURVE ( )  B_SPLINE_CURVE ( 2, ( #8036, #98, #3066, #11031, #2083, #10052, #4111 ),
 .UNSPECIFIED., .F., .F. ) 
 B_SPLINE_CURVE_WITH_KNOTS ( ( 3, 2, 2, 3 ),
 ( 0.5000000000000001110, 0.5333333333333334370, 0.5666666666666666519, 0.5999999999999999778 ),
 .UNSPECIFIED. ) 
 CURVE ( )  GEOMETRIC_REPRESENTATION_ITEM ( )  RATIONAL_B_SPLINE_CURVE ( ( 0.9999999999999995559, 0.8660254037844391517, 1.000000000000000000, 0.8660254037844387076, 1.000000000000000000, 0.8660254037844387076, 1.000000000000000000 ) ) 
 REPRESENTATION_ITEM ( '' )  );
#6914 = CARTESIAN_POINT ( 'NONE',  ( 30.00000000000000711, 121.2009999999999934, -1.499999999999999778 ) ) ;
#6915 = EDGE_LOOP ( 'NONE', ( #11497, #546, #9411, #3617 ) ) ;
#6916 = DIRECTION ( 'NONE',  ( 0.000000000000000000, -0.5150380737757271898, -0.8571673013836847987 ) ) ;
#6917 = LINE ( 'NONE', #9739, #616 ) ;
#6918 = ADVANCED_FACE ( 'NONE', ( #2902 ), #8764, .F. ) ;
#6919 = ORIENTED_EDGE ( 'NONE', *, *, #5347, .T. ) ;
#6920 = CARTESIAN_POINT ( 'NONE',  ( 35.00000000000000000, 90.00000000000000000, -1.000000000000000000 ) ) ;
#6921 = EDGE_CURVE ( 'NONE', #242, #8640, #7717, .T. ) ;
#6922 = VERTEX_POINT ( 'NONE', #5893 ) ;
#6923 = VECTOR ( 'NONE', #6143, 1000.000000000000000 ) ;
#6924 = CARTESIAN_POINT ( 'NONE',  ( 31.50000000000000000, 90.00000000000000000, -3.000000000000000888 ) ) ;
#6925 = ORIENTED_EDGE ( 'NONE', *, *, #2532, .T. ) ;
#6926 = FACE_OUTER_BOUND ( 'NONE', #9289, .T. ) ;
#6927 = CARTESIAN_POINT ( 'NONE',  ( 1.649999999999999911, 0.000000000000000000, 0.000000000000000000 ) ) ;
#6928 = ORIENTED_EDGE ( 'NONE', *, *, #2166, .T. ) ;
#6929 = ORIENTED_EDGE ( 'NONE', *, *, #5975, .T. ) ;
#6930 = AXIS2_PLACEMENT_3D ( 'NONE', #9997, #8947, #1027 ) ;
#6931 = FACE_BOUND ( 'NONE', #652, .T. ) ;
#6932 = ORIENTED_EDGE ( 'NONE', *, *, #11469, .T. ) ;
#6933 = DIRECTION ( 'NONE',  ( 0.000000000000000000, -0.000000000000000000, -1.000000000000000000 ) ) ;
#6934 = ADVANCED_FACE ( 'NONE', ( #12777 ), #4922, .T. ) ;
#6935 = ORIENTED_EDGE ( 'NONE', *, *, #12308, .F. ) ;
#6936 = CARTESIAN_POINT ( 'NONE',  ( 66.44356964374998142, 108.1539533981018053, 3.265625000614516882 ) ) ;
#6937 = ORIENTED_EDGE ( 'NONE', *, *, #3301, .T. ) ;
#6938 = FACE_OUTER_BOUND ( 'NONE', #8192, .T. ) ;
#6939 = CARTESIAN_POINT ( 'NONE',  ( 19.27821517812503060, 62.76906990284727783, 3.528125000614517059 ) ) ;
#6940 = DIRECTION ( 'NONE',  ( 0.000000000000000000, 0.000000000000000000, -1.000000000000000000 ) ) ;
#6941 = VECTOR ( 'NONE', #11053, 1000.000000000000000 ) ;
#6942 = CARTESIAN_POINT ( 'NONE',  ( 66.44356964374998142, 108.1539533981018053, 4.165625000614516793 ) ) ;
#6943 = ADVANCED_FACE ( 'NONE', ( #7798 ), #5710, .T. ) ;
#6944 = PLANE ( 'NONE',  #384 ) ;
#6945 = B_SPLINE_CURVE_WITH_KNOTS ( 'NONE', 3,
 ( #6900, #1006, #12860, #8802 ),
 .UNSPECIFIED., .F., .F.,
 ( 4, 4 ),
 ( 0.000000000000000000, 1.000000000000000000 ),
 .UNSPECIFIED. ) ;
#6946 = ORIENTED_EDGE ( 'NONE', *, *, #11735, .F. ) ;
#6947 = DIRECTION ( 'NONE',  ( -1.000000000000000000, -0.000000000000000000, -0.000000000000000000 ) ) ;
#6948 = CARTESIAN_POINT ( 'NONE',  ( 35.00000000000000000, 90.00000000000000000, 1.000000000000003553 ) ) ;
#6949 = PLANE ( 'NONE',  #9499 ) ;
#6950 = ORIENTED_EDGE ( 'NONE', *, *, #9902, .T. ) ;
#6951 = AXIS2_PLACEMENT_3D ( 'NONE', #9469, #11430, #10707 ) ;
#6952 = CARTESIAN_POINT ( 'NONE',  ( 50.00000000000000000, 0.000000000000000000, 10.00000000000000000 ) ) ;
#6953 = ORIENTED_EDGE ( 'NONE', *, *, #10948, .F. ) ;
#6954 = DIRECTION ( 'NONE',  ( 0.000000000000000000, 0.000000000000000000, 1.000000000000000000 ) ) ;
#6955 = CARTESIAN_POINT ( 'NONE',  ( 3.556430356250015024, 90.00000000000000000, 3.959375000614517415 ) ) ;
#6956 = ORIENTED_EDGE ( 'NONE', *, *, #10868, .F. ) ;
#6957 = CARTESIAN_POINT ( 'NONE',  ( 66.44356964374999563, 90.00000000000000000, 4.634375000614516793 ) ) ;
#6958 = DIRECTION ( 'NONE',  ( -1.000000000000000000, 0.000000000000000000, 0.000000000000000000 ) ) ;
#6959 = ADVANCED_FACE ( 'NONE', ( #6813 ), #10018, .F. ) ;
#6960 = EDGE_CURVE ( 'NONE', #6922, #9462, #6223, .T. ) ;
#6961 = PRESENTATION_LAYER_ASSIGNMENT (  '', '', ( #8836 ) ) ;
#6962 = DIRECTION ( 'NONE',  ( -1.000000000000000000, 0.000000000000000000, 0.000000000000000000 ) ) ;
#6963 = VECTOR ( 'NONE', #8181, 1000.000000000000000 ) ;
#6964 = DIRECTION ( 'NONE',  ( -0.000000000000000000, 1.000000000000000000, -0.000000000000000000 ) ) ;
#6965 = DIRECTION ( 'NONE',  ( 1.000000000000000000, 0.000000000000000000, 5.337610695313252124E-17 ) ) ;
#6966 = CARTESIAN_POINT ( 'NONE',  ( 66.19999999999998863, 90.00000000000000000, 5.000000000000000000 ) ) ;
#6967 = DIRECTION ( 'NONE',  ( -0.000000000000000000, 1.000000000000000000, -0.000000000000000000 ) ) ;
#6968 = ORIENTED_EDGE ( 'NONE', *, *, #2697, .T. ) ;
#6969 = CARTESIAN_POINT ( 'NONE',  ( 64.31840976852106451, 100.6710284717588024, 2.999476386674974737 ) ) ;
#6970 = ORIENTED_EDGE ( 'NONE', *, *, #5393, .T. ) ;
#6971 = DIRECTION ( 'NONE',  ( 1.000000000000000000, -0.000000000000000000, -0.000000000000000000 ) ) ;
#6972 = PRODUCT_RELATED_PRODUCT_CATEGORY ( 'part', '', ( #12209 ) ) ;
#6973 = PRESENTATION_LAYER_ASSIGNMENT (  '', '', ( #8444 ) ) ;
#6974 = CARTESIAN_POINT ( 'NONE',  ( 34.25000000000000000, 92.49999999999998579, -4.802775637732004554 ) ) ;
#6975 = CARTESIAN_POINT ( 'NONE',  ( 17.26299177799148055, 43.12143982588584379, 1.000000000000003109 ) ) ;
#6976 = EDGE_CURVE ( 'NONE', #9073, #10434, #11255, .T. ) ;
#6977 = DIRECTION ( 'NONE',  ( -1.000000000000000000, 0.000000000000000000, 0.000000000000000000 ) ) ;
#6978 = ORIENTED_EDGE ( 'NONE', *, *, #12357, .F. ) ;
#6979 = AXIS2_PLACEMENT_3D ( 'NONE', #12001, #7753, #1805 ) ;
#6980 = DIRECTION ( 'NONE',  ( 0.5000000000000049960, -0.8660254037844357100, 0.000000000000000000 ) ) ;
#6981 = CARTESIAN_POINT ( 'NONE',  ( 1.040000000000000036, 0.5773502691896263972, -1.000000000000000000 ) ) ;
#6982 = VECTOR ( 'NONE', #3261, 1000.000000000000000 ) ;
#6983 = EDGE_LOOP ( 'NONE', ( #9888, #2503, #5088, #10312 ) ) ;
#6984 = DIRECTION ( 'NONE',  ( 0.000000000000000000, 0.000000000000000000, -1.000000000000000000 ) ) ;
#6985 = ORIENTED_EDGE ( 'NONE', *, *, #1995, .F. ) ;
#6986 = DIRECTION ( 'NONE',  ( -1.000000000000000000, 0.000000000000000000, 0.000000000000000000 ) ) ;
#6987 = VERTEX_POINT ( 'NONE', #1251 ) ;
#6988 = FACE_BOUND ( 'NONE', #9654, .T. ) ;
#6989 = CYLINDRICAL_SURFACE ( 'NONE', #4574, 1.599999999999992095 ) ;
#6990 = EDGE_CURVE ( 'NONE', #8977, #11619, #9247, .T. ) ;
#6991 = CIRCLE ( 'NONE', #7822, 3.350000000000000089 ) ;
#6992 = EDGE_LOOP ( 'NONE', ( #12482, #12948, #3471, #3067 ) ) ;
#6993 = EDGE_CURVE ( 'NONE', #10328, #11446, #6880, .T. ) ;
#6994 = AXIS2_PLACEMENT_3D ( 'NONE', #9248, #10232, #3377 ) ;
#6995 =( BOUNDED_CURVE ( )  B_SPLINE_CURVE ( 2, ( #1897, #3680, #6863, #4718, #11646, #3867, #6670 ),
 .UNSPECIFIED., .F., .F. ) 
 B_SPLINE_CURVE_WITH_KNOTS ( ( 3, 2, 2, 3 ),
 ( 0.7000000000000001776, 0.7333333333333335036, 0.7666666666666669405, 0.8000000000000002665 ),
 .UNSPECIFIED. ) 
 CURVE ( )  GEOMETRIC_REPRESENTATION_ITEM ( )  RATIONAL_B_SPLINE_CURVE ( ( 0.9999999999999991118, 0.8660254037844395958, 1.000000000000000000, 0.8660254037844387076, 1.000000000000000000, 0.8660254037844378194, 1.000000000000000888 ) ) 
 REPRESENTATION_ITEM ( '' )  );
#6996 = ADVANCED_FACE ( 'NONE', ( #11195, #8063 ), #10146, .F. ) ;
#6997 = VERTEX_POINT ( 'NONE', #11980 ) ;
#6998 = CARTESIAN_POINT ( 'NONE',  ( 35.00000000000000000, 90.00000000000000000, 6.000000000000000000 ) ) ;
#6999 = EDGE_LOOP ( 'NONE', ( #524, #2555, #3138, #7430 ) ) ;
#7000 = LINE ( 'NONE', #5700, #1453 ) ;
#7001 = EDGE_LOOP ( 'NONE', ( #1122, #3404, #7125 ) ) ;
#7002 = VECTOR ( 'NONE', #486, 1000.000000000000000 ) ;
#7003 = DIRECTION ( 'NONE',  ( 0.000000000000000000, -1.000000000000000000, 0.000000000000000000 ) ) ;
#7004 = PRODUCT_DEFINITION_SHAPE ( 'NONE', 'NONE',  #12974 ) ;
#7005 = VERTEX_POINT ( 'NONE', #2247 ) ;
#7006 = AXIS2_PLACEMENT_3D ( 'NONE', #570, #8573, #6398 ) ;
#7007 = FACE_OUTER_BOUND ( 'NONE', #8225, .T. ) ;
#7008 = CARTESIAN_POINT ( 'NONE',  ( 5.000000000000004441, 76.58915998087155685, -2.500000000000000000 ) ) ;
#7009 = FACE_OUTER_BOUND ( 'NONE', #4935, .T. ) ;
#7010 = CARTESIAN_POINT ( 'NONE',  ( 19.40000000000000924, 117.0199925980744666, 2.787500001229034297 ) ) ;
#7011 = ADVANCED_FACE ( 'NONE', ( #12049 ), #9230, .T. ) ;
#7012 = AXIS2_PLACEMENT_3D ( 'NONE', #940, #7755, #12003 ) ;
#7013 = CARTESIAN_POINT ( 'NONE',  ( 66.19999999999998863, 90.00000000000000000, 4.325000000000000178 ) ) ;
#7014 = VERTEX_POINT ( 'NONE', #2176 ) ;
#7015 = CARTESIAN_POINT ( 'NONE',  ( 64.31840934454761793, 100.6710296366163249, 2.999476389609550431 ) ) ;
#7016 = LINE ( 'NONE', #3822, #8768 ) ;
#7017 = PLANE ( 'NONE',  #4488 ) ;
#7018 = ORIENTED_EDGE ( 'NONE', *, *, #11454, .F. ) ;
#7019 = FACE_OUTER_BOUND ( 'NONE', #7214, .T. ) ;
#7020 = ORIENTED_EDGE ( 'NONE', *, *, #1724, .F. ) ;
#7021 = DIRECTION ( 'NONE',  ( 0.8090169943749476733, 0.5877852522924726930, 0.000000000000000000 ) ) ;
#7022 = CARTESIAN_POINT ( 'NONE',  ( 35.00000000000000711, 53.69209320379640360, 4.465625000614517504 ) ) ;
#7023 = ORIENTED_EDGE ( 'NONE', *, *, #663, .F. ) ;
#7024 = VECTOR ( 'NONE', #5216, 1000.000000000000000 ) ;
#7025 = CARTESIAN_POINT ( 'NONE',  ( 35.00000000000000000, 126.3079067962035822, 4.746875000614517504 ) ) ;
#7026 = FACE_OUTER_BOUND ( 'NONE', #11313, .T. ) ;
#7027 = ADVANCED_FACE ( 'NONE', ( #3161, #8191 ), #9955, .T. ) ;
#7028 = CARTESIAN_POINT ( 'NONE',  ( 40.00000000000000000, 2.000000000000000000, 10.00000000000000000 ) ) ;
#7029 = CARTESIAN_POINT ( 'NONE',  ( -61.00000000000000711, 31.73205080756887142, 3.000000000000000000 ) ) ;
#7030 = CARTESIAN_POINT ( 'NONE',  ( 31.72849223410691266, 88.75612020769642641, 4.800000000000000711 ) ) ;
#7031 = AXIS2_PLACEMENT_3D ( 'NONE', #1455, #5442, #459 ) ;
#7032 = DIRECTION ( 'NONE',  ( 1.000000000000000000, 0.000000000000000000, 0.000000000000000000 ) ) ;
#7033 = ADVANCED_FACE ( 'NONE', ( #251 ), #7995, .T. ) ;
#7034 = EDGE_CURVE ( 'NONE', #11221, #3280, #10226, .T. ) ;
#7035 = CARTESIAN_POINT ( 'NONE',  ( 1.040000000000000036, 0.5773502691896262862, 1.000000000000000000 ) ) ;
#7036 = CARTESIAN_POINT ( 'NONE',  ( 15.49247080330699866, 64.00084030896054799, 1.000000000000003109 ) ) ;
#7037 = ORIENTED_EDGE ( 'NONE', *, *, #9057, .T. ) ;
#7038 = CARTESIAN_POINT ( 'NONE',  ( -56.80384757729341771, 34.46410161513777837, 0.000000000000000000 ) ) ;
#7039 = VERTEX_POINT ( 'NONE', #6021 ) ;
#7040 = VECTOR ( 'NONE', #1277, 1000.000000000000000 ) ;
#7041 = LINE ( 'NONE', #8935, #9880 ) ;
#7042 = LINE ( 'NONE', #11023, #5388 ) ;
#7043 = CARTESIAN_POINT ( 'NONE',  ( -60.00000000000000000, 30.00000000000000000, -10.00000000000000355 ) ) ;
#7044 = DIRECTION ( 'NONE',  ( -1.000000000000000000, 0.000000000000000000, 0.000000000000000000 ) ) ;
#7045 = VERTEX_POINT ( 'NONE', #4982 ) ;
#7046 = CARTESIAN_POINT ( 'NONE',  ( -67.46410161513773573, 36.92820323027551410, 2.500000000000000000 ) ) ;
#7047 = CARTESIAN_POINT ( 'NONE',  ( 25.00000000000000355, 0.000000000000000000, 5.750000000000000000 ) ) ;
#7048 = CIRCLE ( 'NONE', #3092, 6.499999999999999112 ) ;
#7049 = ORIENTED_EDGE ( 'NONE', *, *, #9072, .F. ) ;
#7050 = FACE_OUTER_BOUND ( 'NONE', #5342, .T. ) ;
#7051 = ORIENTED_EDGE ( 'NONE', *, *, #5131, .T. ) ;
#7052 = DIRECTION ( 'NONE',  ( 4.336808689942017243E-16, 2.503857664561960972E-16, -1.000000000000000000 ) ) ;
#7053 = EDGE_LOOP ( 'NONE', ( #8164, #6347, #3013, #8169 ) ) ;
#7054 = ADVANCED_FACE ( 'NONE', ( #8969 ), #56, .F. ) ;
#7055 = CARTESIAN_POINT ( 'NONE',  ( 19.99999999999998224, 90.00000000000000000, -8.000000000000000000 ) ) ;
#7056 = FACE_OUTER_BOUND ( 'NONE', #441, .T. ) ;
#7057 = ORIENTED_EDGE ( 'NONE', *, *, #8210, .F. ) ;
#7058 = VECTOR ( 'NONE', #2369, 1000.000000000000227 ) ;
#7059 = EDGE_LOOP ( 'NONE', ( #11310, #12843, #4923, #11651 ) ) ;
#7060 = CARTESIAN_POINT ( 'NONE',  ( 35.00000000000000000, 90.00000000000000000, -1.000000000000000888 ) ) ;
#7061 = ORIENTED_EDGE ( 'NONE', *, *, #7530, .F. ) ;
#7062 = DIRECTION ( 'NONE',  ( 1.000000000000000000, 0.000000000000000000, 0.000000000000000000 ) ) ;
#7063 = CARTESIAN_POINT ( 'NONE',  ( 3.556430356250014579, 108.1539533981018053, 3.865625000614517415 ) ) ;
#7064 = ORIENTED_EDGE ( 'NONE', *, *, #9484, .F. ) ;
#7065 = DIRECTION ( 'NONE',  ( -0.000000000000000000, 1.000000000000000000, -0.000000000000000000 ) ) ;
#7066 = VECTOR ( 'NONE', #11825, 1000.000000000000000 ) ;
#7067 = VERTEX_POINT ( 'NONE', #6087 ) ;
#7068 = CIRCLE ( 'NONE', #6644, 2.849999999999999201 ) ;
#7069 = CYLINDRICAL_SURFACE ( 'NONE', #5, 1.500000000000001332 ) ;
#7070 = CARTESIAN_POINT ( 'NONE',  ( 66.44356964374998142, 108.1539533981018053, 3.265625000614517326 ) ) ;
#7071 = ADVANCED_FACE ( 'NONE', ( #6152 ), #8128, .F. ) ;
#7072 = DIRECTION ( 'NONE',  ( -1.000000000000000000, 0.000000000000000000, 0.000000000000000000 ) ) ;
#7073 = FACE_OUTER_BOUND ( 'NONE', #9663, .T. ) ;
#7074 = SHAPE_REPRESENTATION_RELATIONSHIP ( 'NONE' , 'NONE' ,  #7342, #9016 ) ;
#7075 = DIRECTION ( 'NONE',  ( -0.4991005450470686888, 0.8665440819333538602, -2.925971193658973835E-17 ) ) ;
#7076 = AXIS2_PLACEMENT_3D ( 'NONE', #5423, #6141, #5234 ) ;
#7077 = ORIENTED_EDGE ( 'NONE', *, *, #2035, .T. ) ;
#7078 = CARTESIAN_POINT ( 'NONE',  ( 50.60000000000001563, 62.98000740192552627, 3.350000000000000533 ) ) ;
#7079 = DIRECTION ( 'NONE',  ( -0.000000000000000000, 1.000000000000000000, -0.000000000000000000 ) ) ;
#7080 = CARTESIAN_POINT ( 'NONE',  ( 35.81220618290669933, 121.3442557591098563, 2.999999999999998668 ) ) ;
#7081 = ORIENTED_EDGE ( 'NONE', *, *, #1677, .F. ) ;
#7082 = CARTESIAN_POINT ( 'NONE',  ( 66.19999999999998863, 90.00000000000000000, 3.875000000000000000 ) ) ;
#7083 = ORIENTED_EDGE ( 'NONE', *, *, #8075, .F. ) ;
#7084 = EDGE_CURVE ( 'NONE', #1830, #12608, #1870, .T. ) ;
#7085 = AXIS2_PLACEMENT_3D ( 'NONE', #3248, #3181, #4415 ) ;
#7086 = CARTESIAN_POINT ( 'NONE',  ( 21.49999999999998579, 86.00000000000000000, -10.00000000000000000 ) ) ;
#7087 = UNCERTAINTY_MEASURE_WITH_UNIT (LENGTH_MEASURE( 1.000000000000000082E-05 ), #1952, 'distance_accuracy_value', 'NONE');
#7088 = CARTESIAN_POINT ( 'NONE',  ( 66.44356964374999563, 71.84604660189820891, 4.090625000614517504 ) ) ;
#7089 = VERTEX_POINT ( 'NONE', #10648 ) ;
#7090 = AXIS2_PLACEMENT_3D ( 'NONE', #733, #790, #7676 ) ;
#7091 = CARTESIAN_POINT ( 'NONE',  ( 3.556430356250028790, 71.84604660189818048, 4.446875000614517681 ) ) ;
#7092 = CARTESIAN_POINT ( 'NONE',  ( 6.499999999999998224, 70.70319397786906279, 1.000000000000000000 ) ) ;
#7093 = LINE ( 'NONE', #4346, #10424 ) ;
#7094 = VECTOR ( 'NONE', #973, 1000.000000000000000 ) ;
#7095 = CYLINDRICAL_SURFACE ( 'NONE', #3653, 1.599999999999993872 ) ;
#7096 = DIRECTION ( 'NONE',  ( -0.000000000000000000, 1.000000000000000000, -0.000000000000000000 ) ) ;
#7097 = EDGE_CURVE ( 'NONE', #3601, #9525, #695, .T. ) ;
#7098 = CARTESIAN_POINT ( 'NONE',  ( 19.99999999999998224, 90.00000000000000000, -5.000000000000000000 ) ) ;
#7099 = DIRECTION ( 'NONE',  ( -1.000000000000000000, 0.000000000000000000, -2.891205793294679312E-17 ) ) ;
#7100 = ORIENTED_EDGE ( 'NONE', *, *, #7619, .F. ) ;
#7101 = AXIS2_PLACEMENT_3D ( 'NONE', #11294, #1545, #12407 ) ;
#7102 = DIRECTION ( 'NONE',  ( 0.03100775193798453039, -0.9995191440486532741, 0.000000000000000000 ) ) ;
#7103 = VERTEX_POINT ( 'NONE', #5304 ) ;
#7104 = EDGE_CURVE ( 'NONE', #5295, #5624, #3663, .T. ) ;
#7105 = EDGE_CURVE ( 'NONE', #9809, #3280, #9732, .T. ) ;
#7106 = CARTESIAN_POINT ( 'NONE',  ( 3.000000000000004441, 27.00000000000000000, -2.500000000000000000 ) ) ;
#7107 = CARTESIAN_POINT ( 'NONE',  ( 45.00000000000000000, 0.000000000000000000, -5.750000000000000000 ) ) ;
#7108 = FACE_BOUND ( 'NONE', #10385, .T. ) ;
#7109 = UNCERTAINTY_MEASURE_WITH_UNIT (LENGTH_MEASURE( 1.000000000000000082E-05 ), #5148, 'distance_accuracy_value', 'NONE');
#7110 = VECTOR ( 'NONE', #5064, 1000.000000000000000 ) ;
#7111 = ORIENTED_EDGE ( 'NONE', *, *, #5011, .T. ) ;
#7112 = CARTESIAN_POINT ( 'NONE',  ( 0.000000000000000000, 0.000000000000000000, 0.000000000000000000 ) ) ;
#7113 = CARTESIAN_POINT ( 'NONE',  ( -1.000000000000000000, -5.473461295629626022, 0.000000000000000000 ) ) ;
#7114 = ORIENTED_EDGE ( 'NONE', *, *, #8598, .T. ) ;
#7115 = EDGE_CURVE ( 'NONE', #587, #3489, #6014, .T. ) ;
#7116 = DIRECTION ( 'NONE',  ( -1.000000000000000000, 0.000000000000000000, 0.000000000000000000 ) ) ;
#7117 = ORIENTED_EDGE ( 'NONE', *, *, #2719, .T. ) ;
#7118 = DIRECTION ( 'NONE',  ( -0.9510565162951529761, -0.3090169943749492276, 0.000000000000000000 ) ) ;
#7119 = VERTEX_POINT ( 'NONE', #10522 ) ;
#7120 = DIRECTION ( 'NONE',  ( -1.000000000000000000, 0.000000000000000000, -0.000000000000000000 ) ) ;
#7121 = CIRCLE ( 'NONE', #5245, 0.5999999999999998668 ) ;
#7122 = DIRECTION ( 'NONE',  ( -0.8665440819333538602, -0.4991005450470686888, -4.805464830191153728E-17 ) ) ;
#7123 = ORIENTED_EDGE ( 'NONE', *, *, #12869, .F. ) ;
#7124 = ADVANCED_FACE ( 'NONE', ( #11756 ), #9297, .F. ) ;
#7125 = ORIENTED_EDGE ( 'NONE', *, *, #5797, .F. ) ;
#7126 = CARTESIAN_POINT ( 'NONE',  ( 10.16381611175368604, 72.81849919625140899, 1.000000000000000000 ) ) ;
#7127 = VERTEX_POINT ( 'NONE', #2743 ) ;
#7128 = CARTESIAN_POINT ( 'NONE',  ( 0.000000000000000000, 0.000000000000000000, 0.000000000000000000 ) ) ;
#7129 = CARTESIAN_POINT ( 'NONE',  ( 35.00000000000000000, 126.3079067962035822, 4.240625000614517859 ) ) ;
#7130 = VERTEX_POINT ( 'NONE', #6717 ) ;
#7131 = FACE_BOUND ( 'NONE', #2985, .T. ) ;
#7132 = DIRECTION ( 'NONE',  ( 0.000000000000000000, 1.000000000000000000, 0.000000000000000000 ) ) ;
#7133 = ORIENTED_EDGE ( 'NONE', *, *, #6879, .F. ) ;
#7134 = DIRECTION ( 'NONE',  ( -0.000000000000000000, -0.000000000000000000, -1.000000000000000000 ) ) ;
#7135 = CARTESIAN_POINT ( 'NONE',  ( 66.44356964374999563, 90.00000000000000000, 3.678125000614516971 ) ) ;
#7136 = CARTESIAN_POINT ( 'NONE',  ( 66.19999999999998863, 90.00000000000000000, 3.875000000000000000 ) ) ;
#7137 = CARTESIAN_POINT ( 'NONE',  ( 64.31840935109022439, 100.6710296186405600, 2.661976390793298286 ) ) ;
#7138 = VECTOR ( 'NONE', #6537, 1000.000000000000000 ) ;
#7139 = CARTESIAN_POINT ( 'NONE',  ( 66.19999999999988916, 71.98667160128361786, 4.287500000000000533 ) ) ;
#7140 = EDGE_LOOP ( 'NONE', ( #5217, #8831 ) ) ;
#7141 = CARTESIAN_POINT ( 'NONE',  ( 3.800000000000015365, 90.00000000000000000, 3.650000000000000355 ) ) ;
#7142 = EDGE_CURVE ( 'NONE', #2989, #7686, #7497, .T. ) ;
#7143 = DIRECTION ( 'NONE',  ( -0.000000000000000000, 1.000000000000000000, -0.000000000000000000 ) ) ;
#7144 = DIRECTION ( 'NONE',  ( -0.000000000000000000, -0.000000000000000000, 1.000000000000000000 ) ) ;
#7145 = ORIENTED_EDGE ( 'NONE', *, *, #9208, .F. ) ;
#7146 = CYLINDRICAL_SURFACE ( 'NONE', #54, 1.599999999999993872 ) ;
#7147 = ORIENTED_EDGE ( 'NONE', *, *, #8348, .F. ) ;
#7148 = CIRCLE ( 'NONE', #1508, 0.5999999999999999778 ) ;
#7149 = CARTESIAN_POINT ( 'NONE',  ( 34.25000000000000000, 92.49999999999998579, -3.000000000000000000 ) ) ;
#7150 = CARTESIAN_POINT ( 'NONE',  ( 3.556430356250015024, 90.00000000000000000, 4.803125000614516971 ) ) ;
#7151 = ORIENTED_EDGE ( 'NONE', *, *, #867, .F. ) ;
#7152 = CARTESIAN_POINT ( 'NONE',  ( 64.54728993811707483, 100.7543353701752125, 2.858851390224067313 ) ) ;
#7153 = FACE_OUTER_BOUND ( 'NONE', #6139, .T. ) ;
#7154 = FACE_OUTER_BOUND ( 'NONE', #7558, .T. ) ;
#7155 = ADVANCED_FACE ( 'NONE', ( #567 ), #12307, .T. ) ;
#7156 = CIRCLE ( 'NONE', #1937, 1.599999999999997202 ) ;
#7157 = DIRECTION ( 'NONE',  ( -1.000000000000000000, 0.000000000000000000, -0.000000000000000000 ) ) ;
#7158 = EDGE_CURVE ( 'NONE', #1479, #12851, #4332, .T. ) ;
#7159 = DIRECTION ( 'NONE',  ( 0.8660254037844361541, 0.5000000000000042188, 0.000000000000000000 ) ) ;
#7160 = DIRECTION ( 'NONE',  ( -1.000000000000000000, 0.000000000000000000, 0.000000000000000000 ) ) ;
#7161 = CARTESIAN_POINT ( 'NONE',  ( 20.00000000000000355, 62.64236852357281293, 1.500000000000000444 ) ) ;
#7162 = DIRECTION ( 'NONE',  ( 0.000000000000000000, -1.000000000000000000, 0.000000000000000000 ) ) ;
#7163 = CARTESIAN_POINT ( 'NONE',  ( 66.44356964375000985, 71.84604660189820891, 3.696875000614517237 ) ) ;
#7164 = EDGE_LOOP ( 'NONE', ( #568, #5214, #4868, #4527 ) ) ;
#7165 = COLOUR_RGB ( '',0.8941176470588234615, 0.8941176470588234615, 0.8941176470588234615 ) ;
#7166 = DIRECTION ( 'NONE',  ( -1.000000000000000000, 0.000000000000000000, -0.000000000000000000 ) ) ;
#7167 = VERTEX_POINT ( 'NONE', #8749 ) ;
#7168 = VECTOR ( 'NONE', #2744, 1000.000000000000000 ) ;
#7169 = ADVANCED_FACE ( 'NONE', ( #1691 ), #4764, .T. ) ;
#7170 = DIRECTION ( 'NONE',  ( -0.8660254037844394848, -0.4999999999999984457, -0.000000000000000000 ) ) ;
#7171 = LINE ( 'NONE', #10179, #3480 ) ;
#7172 = FACE_OUTER_BOUND ( 'NONE', #1732, .T. ) ;
#7173 = EDGE_LOOP ( 'NONE', ( #1542, #8505 ) ) ;
#7174 = CARTESIAN_POINT ( 'NONE',  ( 45.00000000000000711, 90.00000000000000000, -18.00000000000000355 ) ) ;
#7175 = CARTESIAN_POINT ( 'NONE',  ( 45.00000000000000000, -5.901290925839664858, 5.750000000000000888 ) ) ;
#7176 = ORIENTED_EDGE ( 'NONE', *, *, #1023, .T. ) ;
#7177 =( LENGTH_UNIT ( ) NAMED_UNIT ( * ) SI_UNIT ( .MILLI., .METRE. ) );
#7178 = AXIS2_PLACEMENT_3D ( 'NONE', #7368, #10379, #155 ) ;
#7179 = CARTESIAN_POINT ( 'NONE',  ( 7.264852530253062213, 98.48596457872582732, 4.000000000000000000 ) ) ;
#7180 = VERTEX_POINT ( 'NONE', #4575 ) ;
#7181 =( REPRESENTATION_RELATIONSHIP ('NONE','NONE', #1997, #9523 ) REPRESENTATION_RELATIONSHIP_WITH_TRANSFORMATION ( #3793 )SHAPE_REPRESENTATION_RELATIONSHIP( ) );
#7182 = DIRECTION ( 'NONE',  ( 0.000000000000000000, -0.000000000000000000, 1.000000000000000000 ) ) ;
#7183 = ORIENTED_EDGE ( 'NONE', *, *, #1153, .F. ) ;
#7184 = CARTESIAN_POINT ( 'NONE',  ( 3.033375984251971413, -3.035766082959412415E-15, 0.000000000000000000 ) ) ;
#7185 = CARTESIAN_POINT ( 'NONE',  ( -9.666666666666658969, 79.07477288111861924, 0.9999999999999997780 ) ) ;
#7186 = DIRECTION ( 'NONE',  ( -1.000000000000000000, 0.000000000000000000, 0.000000000000000000 ) ) ;
#7187 = ORIENTED_EDGE ( 'NONE', *, *, #12676, .T. ) ;
#7188 = EDGE_CURVE ( 'NONE', #8824, #11432, #11631, .T. ) ;
#7189 = ORIENTED_EDGE ( 'NONE', *, *, #12418, .T. ) ;
#7190 = AXIS2_PLACEMENT_3D ( 'NONE', #9392, #414, #2210 ) ;
#7191 = LINE ( 'NONE', #5031, #3678 ) ;
#7192 = ORIENTED_EDGE ( 'NONE', *, *, #8910, .T. ) ;
#7193 = APPLICATION_PROTOCOL_DEFINITION ( 'draft international standard', 'automotive_design', 1998, #2088 ) ;
#7194 = CARTESIAN_POINT ( 'NONE',  ( 35.00000000000000711, 53.69209320379640360, 3.565625000614517592 ) ) ;
#7195 = ORIENTED_EDGE ( 'NONE', *, *, #3696, .F. ) ;
#7196 = CARTESIAN_POINT ( 'NONE',  ( 66.19999999999993179, 71.98667160128364628, 3.500000001229034208 ) ) ;
#7197 = FACE_OUTER_BOUND ( 'NONE', #4360, .T. ) ;
#7198 = EDGE_CURVE ( 'NONE', #3479, #4591, #5680, .T. ) ;
#7199 = VERTEX_POINT ( 'NONE', #7334 ) ;
#7200 = EDGE_CURVE ( 'NONE', #7727, #261, #6848, .T. ) ;
#7201 = CARTESIAN_POINT ( 'NONE',  ( 0.000000000000000000, 0.5773502691896262862, -1.000000000000000000 ) ) ;
#7202 = VECTOR ( 'NONE', #8506, 1000.000000000000000 ) ;
#7203 = CARTESIAN_POINT ( 'NONE',  ( 19.27821517812500574, 117.2309300971526937, 4.278125000614516615 ) ) ;
#7204 = CIRCLE ( 'NONE', #3869, 3.349999999999995204 ) ;
#7205 = CARTESIAN_POINT ( 'NONE',  ( 19.40000000000002700, 62.98000740192551206, 4.625000000000000000 ) ) ;
#7206 = DIRECTION ( 'NONE',  ( -0.000000000000000000, 1.000000000000000000, -0.000000000000000000 ) ) ;
#7207 =( LENGTH_UNIT ( ) NAMED_UNIT ( * ) SI_UNIT ( .MILLI., .METRE. ) );
#7208 = CARTESIAN_POINT ( 'NONE',  ( 7.650000000000000355, 0.000000000000000000, 0.000000000000000000 ) ) ;
#7209 = ORIENTED_EDGE ( 'NONE', *, *, #12475, .T. ) ;
#7210 = CARTESIAN_POINT ( 'NONE',  ( 35.00000000000000711, 53.97334320256736362, 4.662499999999999645 ) ) ;
#7211 = ORIENTED_EDGE ( 'NONE', *, *, #1157, .T. ) ;
#7212 = AXIS2_PLACEMENT_3D ( 'NONE', #10381, #5144, #1414 ) ;
#7213 = DIRECTION ( 'NONE',  ( 0.000000000000000000, -1.000000000000000000, 0.000000000000000000 ) ) ;
#7214 = EDGE_LOOP ( 'NONE', ( #7520, #4860, #2540, #8204 ) ) ;
#7215 = CIRCLE ( 'NONE', #3255, 2.849999999999999645 ) ;
#7216 = PLANE ( 'NONE',  #12188 ) ;
#7217 = VERTEX_POINT ( 'NONE', #10590 ) ;
#7218 = DIRECTION ( 'NONE',  ( 1.000000000000000000, 0.000000000000000000, 0.000000000000000000 ) ) ;
#7219 = CARTESIAN_POINT ( 'NONE',  ( 66.44356964374999563, 71.84604660189820891, 4.540625000614517681 ) ) ;
#7220 = CARTESIAN_POINT ( 'NONE',  ( 66.44356964374999563, 90.00000000000000000, 4.184375000614516615 ) ) ;
#7221 = CARTESIAN_POINT ( 'NONE',  ( 52.49999999999996447, 94.00000000000000000, -10.00000000000000000 ) ) ;
#7222 = AXIS2_PLACEMENT_3D ( 'NONE', #6692, #4546, #10687 ) ;
#7223 = PRODUCT_DEFINITION_SHAPE ( 'NONE', 'NONE',  #12959 ) ;
#7224 = EDGE_CURVE ( 'NONE', #10861, #8585, #5615, .T. ) ;
#7225 = DIRECTION ( 'NONE',  ( 0.000000000000000000, 0.000000000000000000, -1.000000000000000000 ) ) ;
#7226 = PRESENTATION_LAYER_ASSIGNMENT (  '', '', ( #8479 ) ) ;
#7227 = SURFACE_SIDE_STYLE ('',( #2197 ) ) ;
#7228 = DIRECTION ( 'NONE',  ( 1.000000000000000000, 0.000000000000000000, 0.000000000000000000 ) ) ;
#7229 = LINE ( 'NONE', #1269, #4475 ) ;
#7230 = AXIS2_PLACEMENT_3D ( 'NONE', #72, #8004, #7804 ) ;
#7231 = LINE ( 'NONE', #11215, #10567 ) ;
#7232 = VECTOR ( 'NONE', #8299, 1000.000000000000000 ) ;
#7233 = EDGE_CURVE ( 'NONE', #8374, #12039, #12621, .T. ) ;
#7234 = CARTESIAN_POINT ( 'NONE',  ( 1.040000000000000036, -0.8660254037844382635, 0.5000000000000002220 ) ) ;
#7235 = DIRECTION ( 'NONE',  ( 0.8660254037844361541, 0.5000000000000042188, 0.000000000000000000 ) ) ;
#7236 = ORIENTED_EDGE ( 'NONE', *, *, #9746, .T. ) ;
#7237 = DIRECTION ( 'NONE',  ( -0.8660254037844361541, -0.5000000000000042188, 0.000000000000000000 ) ) ;
#7238 = ORIENTED_EDGE ( 'NONE', *, *, #693, .F. ) ;
#7239 = ADVANCED_FACE ( 'NONE', ( #2991 ), #3850, .T. ) ;
#7240 = VECTOR ( 'NONE', #10953, 1000.000000000000000 ) ;
#7241 = CARTESIAN_POINT ( 'NONE',  ( 20.00000000000000355, 2.000000000000001776, 1.500000000000000444 ) ) ;
#7242 = DIRECTION ( 'NONE',  ( 0.000000000000000000, 0.000000000000000000, 1.000000000000000000 ) ) ;
#7243 = DIRECTION ( 'NONE',  ( -0.000000000000000000, 1.000000000000000000, -0.000000000000000000 ) ) ;
#7244 = EDGE_LOOP ( 'NONE', ( #3282, #9518, #12310, #9235 ) ) ;
#7245 = CARTESIAN_POINT ( 'NONE',  ( 10.16381611175368604, 72.81849919625140899, 5.000000000000000000 ) ) ;
#7246 = CARTESIAN_POINT ( 'NONE',  ( 66.19999999999998863, 90.00000000000000000, 3.987500001229034030 ) ) ;
#7247 = ORIENTED_EDGE ( 'NONE', *, *, #794, .F. ) ;
#7248 = DIRECTION ( 'NONE',  ( 0.000000000000000000, 1.000000000000000000, -0.000000000000000000 ) ) ;
#7249 = ORIENTED_EDGE ( 'NONE', *, *, #5737, .F. ) ;
#7250 = EDGE_CURVE ( 'NONE', #9471, #11248, #2012, .T. ) ;
#7251 = AXIS2_PLACEMENT_3D ( 'NONE', #12414, #1552, #1487 ) ;
#7252 = ORIENTED_EDGE ( 'NONE', *, *, #1929, .F. ) ;
#7253 = DIRECTION ( 'NONE',  ( -0.000000000000000000, 0.000000000000000000, 1.000000000000000000 ) ) ;
#7254 = DIRECTION ( 'NONE',  ( 0.000000000000000000, 0.000000000000000000, -1.000000000000000000 ) ) ;
#7255 = EDGE_LOOP ( 'NONE', ( #9563, #8777, #10726, #2700 ) ) ;
#7256 = ORIENTED_EDGE ( 'NONE', *, *, #7600, .F. ) ;
#7257 = AXIS2_PLACEMENT_3D ( 'NONE', #12535, #5524, #1405 ) ;
#7258 = DIRECTION ( 'NONE',  ( 0.4999999999999995559, -0.8660254037844389297, 0.000000000000000000 ) ) ;
#7259 = ORIENTED_EDGE ( 'NONE', *, *, #5161, .F. ) ;
#7260 = PRODUCT_CONTEXT ( 'NONE', #1241, 'mechanical' ) ;
#7261 = CARTESIAN_POINT ( 'NONE',  ( 35.00000000000000711, 53.69209320379640360, 3.115625000614517415 ) ) ;
#7262 = EDGE_LOOP ( 'NONE', ( #11931, #7057, #8489, #7320 ) ) ;
#7263 = FACE_OUTER_BOUND ( 'NONE', #8698, .T. ) ;
#7264 = ORIENTED_EDGE ( 'NONE', *, *, #9805, .T. ) ;
#7265 = EDGE_CURVE ( 'NONE', #427, #10175, #7418, .T. ) ;
#7266 =( BOUNDED_CURVE ( )  B_SPLINE_CURVE ( 2, ( #1196, #9900, #932, #2058, #10031, #1061, #8270, #1262, #12382, #9436, #8335, #8464, #10484, #5255, #2260, #8399, #6422, #1456, #7220, #460, #2324, #6236, #5443, #11208, #2383, #9243, #1520, #2450, #10358, #11331, #6362, #12260, #7412, #3307, #4469, #4282, #10421, #10290, #10228, #12452, #11399, #3499, #7478, #4343, #1390, #11462, #396, #2513, #8205, #265, #6490, #5509, #334, #7285, #12323 ),
 .UNSPECIFIED., .F., .F. ) 
 B_SPLINE_CURVE_WITH_KNOTS ( ( 3, 2, 2, 2, 2, 2, 2, 2, 2, 2, 2, 2, 2, 2, 2, 2, 2, 2, 2, 2, 2, 2, 2, 2, 2, 2, 2, 3 ),
 ( 0.000000000000000000, 0.03333333333333333287, 0.06666666666666666574, 0.1000000000000000056, 0.1333333333333333315, 0.1666666666666666574, 0.2000000000000000111, 0.2333333333333333370, 0.2666666666666666630, 0.2999999999999999889, 0.3333333333333333148, 0.3666666666666666408, 0.4000000000000000222, 0.4333333333333333481, 0.4666666666666666741, 0.5000000000000000000, 0.5333333333333333259, 0.5666666666666666519, 0.5999999999999999778, 0.6333333333333333037, 0.6666666666666666297, 0.6999999999999999556, 0.7333333333333332815, 0.7666666666666667185, 0.8000000000000000444, 0.8333333333333333703, 0.8666666666666666963, 0.8887752010443025208 ),
 .UNSPECIFIED. ) 
 CURVE ( )  GEOMETRIC_REPRESENTATION_ITEM ( )  RATIONAL_B_SPLINE_CURVE ( ( 1.000000000000000000, 0.8660254037844387076, 1.000000000000000000, 0.8660254037844387076, 1.000000000000000000, 0.8660254037844387076, 1.000000000000000000, 0.8660254037844387076, 1.000000000000000000, 0.8660254037844387076, 1.000000000000000000, 0.8660254037844387076, 1.000000000000000000, 0.8660254037844387076, 1.000000000000000000, 0.8660254037844387076, 1.000000000000000000, 0.8660254037844387076, 1.000000000000000000, 0.8660254037844387076, 1.000000000000000000, 0.8660254037844387076, 1.000000000000000000, 0.8660254037844387076, 1.000000000000000000, 0.8660254037844387076, 1.000000000000000000, 0.8660254037844387076, 1.000000000000000000, 0.8660254037844387076, 1.000000000000000000, 0.8660254037844387076, 1.000000000000000000, 0.8660254037844387076, 1.000000000000000000, 0.8660254037844387076, 1.000000000000000000, 0.8660254037844387076, 1.000000000000000000, 0.8660254037844387076, 1.000000000000000000, 0.8660254037844387076, 1.000000000000000000, 0.8660254037844387076, 1.000000000000000000, 0.8660254037844387076, 1.000000000000000000, 0.8660254037844387076, 1.000000000000000000, 0.8660254037844387076, 1.000000000000000000, 0.8660254037844387076, 1.000000000000000000, 0.9111405410151519613, 0.9401542262549813511 ) ) 
 REPRESENTATION_ITEM ( '' )  );
#7267 = LINE ( 'NONE', #8317, #3595 ) ;
#7268 = VECTOR ( 'NONE', #2245, 1000.000000000000000 ) ;
#7269 = PLANE ( 'NONE',  #12790 ) ;
#7270 = CARTESIAN_POINT ( 'NONE',  ( -18.33333333333332504, 46.12451549659709116, 7.999999999999996447 ) ) ;
#7271 = DIRECTION ( 'NONE',  ( -1.000000000000000000, 0.000000000000000000, -0.000000000000000000 ) ) ;
#7272 = EDGE_CURVE ( 'NONE', #9145, #9386, #1001, .T. ) ;
#7274 = EDGE_CURVE ( 'NONE', #7119, #12628, #3916, .T. ) ;
#7273 = ORIENTED_EDGE ( 'NONE', *, *, #4413, .T. ) ;
#7275 = CARTESIAN_POINT ( 'NONE',  ( 66.20000000000000284, 71.98667160128370313, 3.387500000000000178 ) ) ;
#7276 = CIRCLE ( 'NONE', #10194, 31.20000000000000639 ) ;
#7277 = CARTESIAN_POINT ( 'NONE',  ( 1.040000000000000036, -1.154700538379251684, 0.000000000000000000 ) ) ;
#7278 = CIRCLE ( 'NONE', #5192, 1.599999999999986766 ) ;
#7279 = ORIENTED_EDGE ( 'NONE', *, *, #11152, .T. ) ;
#7280 = DIRECTION ( 'NONE',  ( -1.000000000000000000, -0.000000000000000000, -0.000000000000000000 ) ) ;
#7281 = ORIENTED_EDGE ( 'NONE', *, *, #4483, .T. ) ;
#7282 = PLANE ( 'NONE',  #1051 ) ;
#7283 = EDGE_CURVE ( 'NONE', #3861, #1427, #10837, .T. ) ;
#7284 = LINE ( 'NONE', #4150, #4941 ) ;
#7285 = CARTESIAN_POINT ( 'NONE',  ( 60.63303221600038739, 111.5086687461494250, 2.885734441893565538 ) ) ;
#7286 = LINE ( 'NONE', #4283, #561 ) ;
#7288 = AXIS2_PLACEMENT_3D ( 'NONE', #6586, #10589, #5736 ) ;
#7287 = LINE ( 'NONE', #3373, #3325 ) ;
#7289 = CARTESIAN_POINT ( 'NONE',  ( 1.040000000000000036, 0.5773502691896263972, -1.000000000000000000 ) ) ;
#7290 = CARTESIAN_POINT ( 'NONE',  ( 35.00000000000000000, 90.00000000000000000, 6.000000000000000000 ) ) ;
#7291 = DIRECTION ( 'NONE',  ( 0.000000000000000000, 0.000000000000000000, -1.000000000000000000 ) ) ;
#7292 = AXIS2_PLACEMENT_3D ( 'NONE', #1597, #5584, #2456 ) ;
#7293 = CARTESIAN_POINT ( 'NONE',  ( 20.00000000000000355, 0.000000000000000000, -10.00000000000000000 ) ) ;
#7294 = EDGE_CURVE ( 'NONE', #3489, #11952, #8999, .T. ) ;
#7295 = AXIS2_PLACEMENT_3D ( 'NONE', #6365, #10362, #7610 ) ;
#7296 = CARTESIAN_POINT ( 'NONE',  ( 52.49999999999996447, 94.00000000000000000, -8.000000000000000000 ) ) ;
#7297 = CARTESIAN_POINT ( 'NONE',  ( 35.00000000000000000, 126.3079067962036106, 3.396875000614517415 ) ) ;
#7298 = ORIENTED_EDGE ( 'NONE', *, *, #2248, .T. ) ;
#7299 = CARTESIAN_POINT ( 'NONE',  ( 25.00000000000000000, 90.00000000000000000, -18.00000000000000355 ) ) ;
#7300 = ORIENTED_EDGE ( 'NONE', *, *, #322, .F. ) ;
#7301 = AXIS2_PLACEMENT_3D ( 'NONE', #10811, #8912, #12907 ) ;
#7302 = VECTOR ( 'NONE', #5646, 1000.000000000000000 ) ;
#7303 = CYLINDRICAL_SURFACE ( 'NONE', #2691, 31.19999999999999929 ) ;
#7304 = DIRECTION ( 'NONE',  ( -0.000000000000000000, -0.000000000000000000, 1.000000000000000000 ) ) ;
#7305 = DIRECTION ( 'NONE',  ( 0.000000000000000000, -0.000000000000000000, -1.000000000000000000 ) ) ;
#7306 = ORIENTED_EDGE ( 'NONE', *, *, #5565, .F. ) ;
#7307 = DIRECTION ( 'NONE',  ( -1.000000000000000000, 0.000000000000000000, 0.000000000000000000 ) ) ;
#7308 = EDGE_CURVE ( 'NONE', #5354, #10861, #5988, .T. ) ;
#7309 = CARTESIAN_POINT ( 'NONE',  ( 25.00000000000000355, 0.000000000000000000, -5.750000000000000000 ) ) ;
#7310 = VERTEX_POINT ( 'NONE', #2871 ) ;
#7311 = CIRCLE ( 'NONE', #1673, 30.19999999999999218 ) ;
#7312 = CARTESIAN_POINT ( 'NONE',  ( 1.649999999999999911, 3.490243377569955568E-16, -2.849999999999999201 ) ) ;
#7313 = EDGE_LOOP ( 'NONE', ( #657, #3385, #4112, #8855 ) ) ;
#7314 = VERTEX_POINT ( 'NONE', #9917 ) ;
#7315 = CARTESIAN_POINT ( 'NONE',  ( 50.59999999999999432, 117.0199925980744666, 4.512500001229033941 ) ) ;
#7316 = CYLINDRICAL_SURFACE ( 'NONE', #3533, 3.350000000000003642 ) ;
#7317 = ORIENTED_EDGE ( 'NONE', *, *, #136, .F. ) ;
#7318 = AXIS2_PLACEMENT_3D ( 'NONE', #11556, #12737, #2602 ) ;
#7319 = ADVANCED_FACE ( 'NONE', ( #4040 ), #11945, .F. ) ;
#7320 = ORIENTED_EDGE ( 'NONE', *, *, #6357, .T. ) ;
#7321 = CARTESIAN_POINT ( 'NONE',  ( -60.00000000000000000, 0.000000000000000000, 9.999999999999996447 ) ) ;
#7322 = EDGE_LOOP ( 'NONE', ( #7813, #7279, #11627, #1579 ) ) ;
#7323 = EDGE_CURVE ( 'NONE', #12128, #6987, #884, .T. ) ;
#7324 = DIRECTION ( 'NONE',  ( 0.000000000000000000, 0.000000000000000000, 1.000000000000000000 ) ) ;
#7325 = CARTESIAN_POINT ( 'NONE',  ( 35.00000000000000000, 126.0266567974326222, 3.200000001229034385 ) ) ;
#7326 = ORIENTED_EDGE ( 'NONE', *, *, #8839, .T. ) ;
#7327 = DIRECTION ( 'NONE',  ( 0.000000000000000000, 0.000000000000000000, -1.000000000000000000 ) ) ;
#7328 = ORIENTED_EDGE ( 'NONE', *, *, #2086, .F. ) ;
#7329 = AXIS2_PLACEMENT_3D ( 'NONE', #9240, #458, #4466 ) ;
#7330 = CARTESIAN_POINT ( 'NONE',  ( 35.00000000000000000, 90.00000000000000000, 22.38477631085024555 ) ) ;
#7331 = CARTESIAN_POINT ( 'NONE',  ( 3.800000000000015810, 108.0133283987162969, 3.275000001229034563 ) ) ;
#7332 = DIRECTION ( 'NONE',  ( 0.000000000000000000, 0.000000000000000000, 1.000000000000000000 ) ) ;
#7333 = CARTESIAN_POINT ( 'NONE',  ( 25.00000000000000355, 3.649999999999993694, 5.750000000000000000 ) ) ;
#7334 = CARTESIAN_POINT ( 'NONE',  ( 50.09999999999995168, 90.00000000000000000, -10.00000000000000178 ) ) ;
#7335 = EDGE_CURVE ( 'NONE', #5885, #9045, #8812, .T. ) ;
#7336 = VERTEX_POINT ( 'NONE', #8875 ) ;
#7337 = AXIS2_PLACEMENT_3D ( 'NONE', #5641, #7669, #12516 ) ;
#7338 = CARTESIAN_POINT ( 'NONE',  ( 50.72178482187499071, 117.2309300971526937, 3.809375000614517504 ) ) ;
#7339 = EDGE_LOOP ( 'NONE', ( #12515, #1512, #10815 ) ) ;
#7340 = PLANE ( 'NONE',  #11266 ) ;
#7341 = ORIENTED_EDGE ( 'NONE', *, *, #10006, .T. ) ;
#7342 = SHAPE_REPRESENTATION ( 'conveyor wheel', ( #5704 ), #2789 ) ;
#7343 = CYLINDRICAL_SURFACE ( 'NONE', #5072, 0.5999999999999998668 ) ;
#7344 = VERTEX_POINT ( 'NONE', #9065 ) ;
#7345 = CARTESIAN_POINT ( 'NONE',  ( 45.00000000000000000, 0.000000000000000000, -4.249999999999998224 ) ) ;
#7346 = DIRECTION ( 'NONE',  ( -1.000000000000000000, 0.000000000000000000, 0.000000000000000000 ) ) ;
#7347 = EDGE_CURVE ( 'NONE', #6159, #7310, #7042, .T. ) ;
#7348 = CARTESIAN_POINT ( 'NONE',  ( 1.040000000000000036, -0.5773502691896256200, -1.000000000000000000 ) ) ;
#7349 = AXIS2_PLACEMENT_3D ( 'NONE', #2689, #5489, #11513 ) ;
#7350 = CARTESIAN_POINT ( 'NONE',  ( 1.040000000000000036, -0.5773502691896253980, 1.000000000000000000 ) ) ;
#7351 = DIRECTION ( 'NONE',  ( -0.000000000000000000, -0.000000000000000000, -1.000000000000000000 ) ) ;
#7352 = CARTESIAN_POINT ( 'NONE',  ( 1.040000000000000036, -0.5773502691896253980, 1.000000000000000000 ) ) ;
#7353 = DIRECTION ( 'NONE',  ( -0.000000000000000000, 1.000000000000000000, -0.000000000000000000 ) ) ;
#7354 = DIRECTION ( 'NONE',  ( -0.5000000000000036637, 0.8660254037844365982, 0.000000000000000000 ) ) ;
#7355 = DIRECTION ( 'NONE',  ( -1.000000000000000000, 0.000000000000000000, 0.000000000000000000 ) ) ;
#7356 = AXIS2_PLACEMENT_3D ( 'NONE', #9372, #4408, #3429 ) ;
#7357 = CARTESIAN_POINT ( 'NONE',  ( 9.650000000000000355, 0.000000000000000000, 0.000000000000000000 ) ) ;
#7358 = DIRECTION ( 'NONE',  ( 1.000000000000000000, 0.000000000000000000, 0.000000000000000000 ) ) ;
#7359 = CARTESIAN_POINT ( 'NONE',  ( 1.000000000000000000, -5.473461295629626022, -0.8000000000000000444 ) ) ;
#7361 = EDGE_CURVE ( 'NONE', #11555, #12599, #3521, .T. ) ;
#7360 = ORIENTED_EDGE ( 'NONE', *, *, #9982, .F. ) ;
#7362 = EDGE_CURVE ( 'NONE', #3514, #3599, #7831, .T. ) ;
#7363 = LINE ( 'NONE', #8155, #1407 ) ;
#7364 = ORIENTED_EDGE ( 'NONE', *, *, #11382, .T. ) ;
#7365 = AXIS2_PLACEMENT_3D ( 'NONE', #8825, #8952, #1958 ) ;
#7366 = LINE ( 'NONE', #2402, #8968 ) ;
#7367 = CARTESIAN_POINT ( 'NONE',  ( 3.800000000000039790, 71.98667160128364628, 4.250000001229034652 ) ) ;
#7368 = CARTESIAN_POINT ( 'NONE',  ( 20.20191803945384379, 39.07635485401110742, 1.000000000000003109 ) ) ;
#7369 = VERTEX_POINT ( 'NONE', #11886 ) ;
#7370 = DIRECTION ( 'NONE',  ( 0.000000000000000000, 0.000000000000000000, 1.000000000000000000 ) ) ;
#7371 = CARTESIAN_POINT ( 'NONE',  ( -60.00000000000000000, 0.000000000000000000, -15.00000000000000355 ) ) ;
#7372 = ORIENTED_EDGE ( 'NONE', *, *, #2518, .T. ) ;
#7373 = CARTESIAN_POINT ( 'NONE',  ( 0.000000000000000000, 0.000000000000000000, 0.000000000000000000 ) ) ;
#7374 = CARTESIAN_POINT ( 'NONE',  ( 35.00000000000000000, 90.00000000000000000, -10.00000000000000000 ) ) ;
#7375 = ORIENTED_EDGE ( 'NONE', *, *, #1077, .F. ) ;
#7376 = VERTEX_POINT ( 'NONE', #10896 ) ;
#7377 = CARTESIAN_POINT ( 'NONE',  ( 64.31840935109022439, 100.6710296186405742, 2.661976390793298286 ) ) ;
#7378 = DIRECTION ( 'NONE',  ( 4.336808689942017243E-16, 0.000000000000000000, 1.000000000000000000 ) ) ;
#7379 = EDGE_CURVE ( 'NONE', #9156, #4442, #7276, .T. ) ;
#7380 = ORIENTED_EDGE ( 'NONE', *, *, #6771, .F. ) ;
#7381 = PRESENTATION_LAYER_ASSIGNMENT (  '', '', ( #268 ) ) ;
#7382 = ORIENTED_EDGE ( 'NONE', *, *, #976, .T. ) ;
#7383 = PLANE ( 'NONE',  #7006 ) ;
#7384 = VERTEX_POINT ( 'NONE', #10778 ) ;
#7385 = AXIS2_PLACEMENT_3D ( 'NONE', #10284, #1316, #5312 ) ;
#7386 = CARTESIAN_POINT ( 'NONE',  ( -4.338286831716297698, 0.4117131682837010809, -0.8000000000000000444 ) ) ;
#7387 = CARTESIAN_POINT ( 'NONE',  ( 50.60000000000001563, 62.98000740192552627, 3.350000000000000533 ) ) ;
#7388 = ORIENTED_EDGE ( 'NONE', *, *, #4879, .T. ) ;
#7389 = DIRECTION ( 'NONE',  ( -0.000000000000000000, 1.000000000000000000, -0.000000000000000000 ) ) ;
#7390 = ORIENTED_EDGE ( 'NONE', *, *, #4273, .T. ) ;
#7391 =( GEOMETRIC_REPRESENTATION_CONTEXT ( 3 ) GLOBAL_UNCERTAINTY_ASSIGNED_CONTEXT ( ( #9174 ) ) GLOBAL_UNIT_ASSIGNED_CONTEXT ( ( #9424, #1310, #12178 ) ) REPRESENTATION_CONTEXT ( 'NONE', 'WORKASPACE' ) );
#7392 = EDGE_CURVE ( 'NONE', #9125, #191, #11870, .T. ) ;
#7393 = CARTESIAN_POINT ( 'NONE',  ( 1.040000000000000036, 0.5773502691896263972, 1.000000000000000000 ) ) ;
#7394 = EDGE_LOOP ( 'NONE', ( #6089, #2288, #7133, #10156, #4726, #1176 ) ) ;
#7395 = ADVANCED_FACE ( 'NONE', ( #11223 ), #7303, .F. ) ;
#7396 = DIRECTION ( 'NONE',  ( -1.000000000000000000, 0.000000000000000000, -0.000000000000000000 ) ) ;
#7397 = FACE_OUTER_BOUND ( 'NONE', #1417, .T. ) ;
#7398 = AXIS2_PLACEMENT_3D ( 'NONE', #1612, #12669, #8552 ) ;
#7399 = EDGE_CURVE ( 'NONE', #3015, #2762, #9129, .T. ) ;
#7400 = ORIENTED_EDGE ( 'NONE', *, *, #7737, .F. ) ;
#7401 = PRODUCT_DEFINITION_FORMATION_WITH_SPECIFIED_SOURCE ( 'ANY', '', #12209, .NOT_KNOWN. ) ;
#7402 = CARTESIAN_POINT ( 'NONE',  ( 50.72178482187501203, 62.76906990284730625, 3.209375000614517415 ) ) ;
#7403 = ORIENTED_EDGE ( 'NONE', *, *, #11304, .T. ) ;
#7404 = CARTESIAN_POINT ( 'NONE',  ( 34.25000000000000000, 93.50000000000000000, 4.000000000000000000 ) ) ;
#7405 = VECTOR ( 'NONE', #2457, 1000.000000000000000 ) ;
#7406 = CARTESIAN_POINT ( 'NONE',  ( 35.00000000000000000, 126.3079067962035822, 2.946875000614516793 ) ) ;
#7407 = ORIENTED_EDGE ( 'NONE', *, *, #2025, .F. ) ;
#7408 = CIRCLE ( 'NONE', #10541, 28.99999999999999289 ) ;
#7409 = FACE_OUTER_BOUND ( 'NONE', #6882, .T. ) ;
#7410 = LINE ( 'NONE', #12584, #1182 ) ;
#7411 = EDGE_CURVE ( 'NONE', #4019, #6792, #6380, .T. ) ;
#7412 = CARTESIAN_POINT ( 'NONE',  ( 50.72178482187501203, 62.76906990284730625, 3.659375000614517592 ) ) ;
#7413 = CARTESIAN_POINT ( 'NONE',  ( 25.00000000000000355, -5.000000000000000000, -5.750000000000000000 ) ) ;
#7414 = CARTESIAN_POINT ( 'NONE',  ( 35.00000000000000000, 90.00000000000000000, 6.000000000000000000 ) ) ;
#7415 = CIRCLE ( 'NONE', #8468, 1.000000000000000000 ) ;
#7416 = PLANE ( 'NONE',  #12946 ) ;
#7417 = AXIS2_PLACEMENT_3D ( 'NONE', #8147, #3179, #6241 ) ;
#7418 =( BOUNDED_CURVE ( )  B_SPLINE_CURVE ( 2, ( #2078, #1014, #12873, #5012, #3979, #1941, #4105 ),
 .UNSPECIFIED., .F., .F. ) 
 B_SPLINE_CURVE_WITH_KNOTS ( ( 3, 2, 2, 3 ),
 ( 0.5999999999999999778, 0.6333333333333334147, 0.6666666666666667407, 0.7000000000000001776 ),
 .UNSPECIFIED. ) 
 CURVE ( )  GEOMETRIC_REPRESENTATION_ITEM ( )  RATIONAL_B_SPLINE_CURVE ( ( 1.000000000000000000, 0.8660254037844387076, 1.000000000000000000, 0.8660254037844387076, 1.000000000000000000, 0.8660254037844378194, 1.000000000000000888 ) ) 
 REPRESENTATION_ITEM ( '' )  );
#7419 = DIRECTION ( 'NONE',  ( 0.4719909656437442647, -0.8816033849473842166, 2.775557561595757269E-17 ) ) ;
#7420 = DIRECTION ( 'NONE',  ( -1.000000000000000000, 0.000000000000000000, 0.000000000000000000 ) ) ;
#7421 = CARTESIAN_POINT ( 'NONE',  ( 60.00000000000000000, 0.000000000000000000, -15.00000000000000355 ) ) ;
#7422 = CYLINDRICAL_SURFACE ( 'NONE', #7222, 1.599999999999990319 ) ;
#7423 = CARTESIAN_POINT ( 'NONE',  ( 9.999999999999994671, 27.00000000000000000, -2.500000000000000000 ) ) ;
#7424 = VECTOR ( 'NONE', #3857, 1000.000000000000000 ) ;
#7425 = DIRECTION ( 'NONE',  ( -0.000000000000000000, -0.000000000000000000, -1.000000000000000000 ) ) ;
#7426 = ORIENTED_EDGE ( 'NONE', *, *, #11796, .F. ) ;
#7427 = EDGE_CURVE ( 'NONE', #6795, #12707, #7366, .T. ) ;
#7428 = CIRCLE ( 'NONE', #12445, 30.00000000000000000 ) ;
#7429 = CARTESIAN_POINT ( 'NONE',  ( -31.49999999999998579, 48.76388374866304076, 3.000000000000000000 ) ) ;
#7430 = ORIENTED_EDGE ( 'NONE', *, *, #5057, .T. ) ;
#7431 =( LENGTH_UNIT ( ) NAMED_UNIT ( * ) SI_UNIT ( .MILLI., .METRE. ) );
#7432 = CARTESIAN_POINT ( 'NONE',  ( -60.00000000000000000, 30.00000000000000000, 9.999999999999996447 ) ) ;
#7433 = FACE_OUTER_BOUND ( 'NONE', #1041, .T. ) ;
#7434 = VECTOR ( 'NONE', #6305, 1000.000000000000000 ) ;
#7435 = EDGE_CURVE ( 'NONE', #11750, #10649, #5333, .T. ) ;
#7436 = PLANE ( 'NONE',  #7398 ) ;
#7437 = EDGE_CURVE ( 'NONE', #6538, #4251, #2140, .T. ) ;
#7438 = EDGE_LOOP ( 'NONE', ( #7317, #9649, #164, #5664 ) ) ;
#7439 = CARTESIAN_POINT ( 'NONE',  ( 7.500000000000000000, 34.99999999999999289, 1.499999999999999556 ) ) ;
#7440 = CARTESIAN_POINT ( 'NONE',  ( 3.556430356250015024, 90.00000000000000000, 4.803125000614516971 ) ) ;
#7441 = ORIENTED_EDGE ( 'NONE', *, *, #9262, .F. ) ;
#7442 = DIRECTION ( 'NONE',  ( 1.000000000000000000, 0.000000000000000000, 0.000000000000000000 ) ) ;
#7443 = PLANE ( 'NONE',  #7655 ) ;
#7444 = ORIENTED_EDGE ( 'NONE', *, *, #2066, .T. ) ;
#7445 = DIRECTION ( 'NONE',  ( 0.000000000000000000, 0.000000000000000000, 1.000000000000000000 ) ) ;
#7446 = ORIENTED_EDGE ( 'NONE', *, *, #9188, .F. ) ;
#7447 = EDGE_CURVE ( 'NONE', #6762, #8980, #1343, .T. ) ;
#7448 = CARTESIAN_POINT ( 'NONE',  ( 0.000000000000000000, 0.000000000000000000, 2.849999999999999645 ) ) ;
#7449 = FACE_OUTER_BOUND ( 'NONE', #8357, .T. ) ;
#7450 = ORIENTED_EDGE ( 'NONE', *, *, #10761, .T. ) ;
#7451 = VERTEX_POINT ( 'NONE', #11088 ) ;
#7452 = CARTESIAN_POINT ( 'NONE',  ( 35.75000000000000711, 93.26496554346289258, 4.000000000000000000 ) ) ;
#7453 = EDGE_LOOP ( 'NONE', ( #3332, #4035 ) ) ;
#7454 = CARTESIAN_POINT ( 'NONE',  ( 4.270088556250601699E-16, 2.000000000000000000, -8.000000000000000000 ) ) ;
#7455 = APPLICATION_PROTOCOL_DEFINITION ( 'draft international standard', 'automotive_design', 1998, #11442 ) ;
#7456 = CARTESIAN_POINT ( 'NONE',  ( 35.00000000000000000, 126.0266567974326222, 4.550000001229034474 ) ) ;
#7457 = CONICAL_SURFACE ( 'NONE', #1814, 1.219500000000000028, 0.7853981633974463916 ) ;
#7458 = ORIENTED_EDGE ( 'NONE', *, *, #12524, .F. ) ;
#7459 = EDGE_CURVE ( 'NONE', #11940, #6159, #8536, .T. ) ;
#7460 = VERTEX_POINT ( 'NONE', #8354 ) ;
#7461 =( LENGTH_UNIT ( ) NAMED_UNIT ( * ) SI_UNIT ( .MILLI., .METRE. ) );
#7462 = ORIENTED_EDGE ( 'NONE', *, *, #11466, .F. ) ;
#7463 = CARTESIAN_POINT ( 'NONE',  ( 3.800000000000015365, 90.00000000000000000, 3.312500001229034652 ) ) ;
#7464 = DIRECTION ( 'NONE',  ( -1.000000000000000000, 0.000000000000000000, -0.000000000000000000 ) ) ;
#7465 = AXIS2_PLACEMENT_3D ( 'NONE', #2207, #12273, #11149 ) ;
#7466 = ORIENTED_EDGE ( 'NONE', *, *, #7830, .T. ) ;
#7467 = CARTESIAN_POINT ( 'NONE',  ( 35.00000000000000000, 126.3079067962035822, 4.296875000614517326 ) ) ;
#7468 = ADVANCED_FACE ( 'NONE', ( #12146 ), #1423, .F. ) ;
#7469 = EDGE_LOOP ( 'NONE', ( #2929, #909, #12753, #7147, #8958 ) ) ;
#7470 = CARTESIAN_POINT ( 'NONE',  ( 35.00000000000000711, 53.97334320256736362, 2.975000001229034297 ) ) ;
#7471 = ORIENTED_EDGE ( 'NONE', *, *, #531, .F. ) ;
#7472 = CARTESIAN_POINT ( 'NONE',  ( 3.556430356250014579, 108.1539533981018053, 3.921875000614517326 ) ) ;
#7473 = ADVANCED_FACE ( 'NONE', ( #1410 ), #10376, .F. ) ;
#7474 = ORIENTED_EDGE ( 'NONE', *, *, #4943, .F. ) ;
#7475 = CIRCLE ( 'NONE', #10186, 6.450000000000001066 ) ;
#7476 = CARTESIAN_POINT ( 'NONE',  ( 6.499999999999999112, 68.39379290111055809, -1.000000000000000222 ) ) ;
#7477 = CARTESIAN_POINT ( 'NONE',  ( -3.666666666666661634, 79.07477288111861924, -1.000000000000000666 ) ) ;
#7478 = CARTESIAN_POINT ( 'NONE',  ( 66.44356964374999563, 90.00000000000000000, 3.284375000614517148 ) ) ;
#7479 = DIRECTION ( 'NONE',  ( -0.000000000000000000, -0.000000000000000000, -1.000000000000000000 ) ) ;
#7480 = CARTESIAN_POINT ( 'NONE',  ( -31.49999999999998579, 48.76388374866304076, -1.000000000000000000 ) ) ;
#7481 = FACE_OUTER_BOUND ( 'NONE', #1419, .T. ) ;
#7482 = CIRCLE ( 'NONE', #991, 1.500000000000001332 ) ;
#7483 = DIRECTION ( 'NONE',  ( 0.000000000000000000, 0.000000000000000000, 1.000000000000000000 ) ) ;
#7484 = ADVANCED_FACE ( 'NONE', ( #9330 ), #4172, .F. ) ;
#7485 = CARTESIAN_POINT ( 'NONE',  ( 1.749999999999999112, 0.000000000000000000, 0.000000000000000000 ) ) ;
#7486 = DIRECTION ( 'NONE',  ( 0.8660254037844400399, 0.000000000000000000, -0.4999999999999975575 ) ) ;
#7487 = LINE ( 'NONE', #8604, #10775 ) ;
#7488 = ADVANCED_FACE ( 'NONE', ( #4427 ), #10946, .F. ) ;
#7489 = CARTESIAN_POINT ( 'NONE',  ( 48.49999999999995737, 90.00000000000000000, -10.00000000000000000 ) ) ;
#7490 = DIRECTION ( 'NONE',  ( 0.000000000000000000, 0.000000000000000000, 1.000000000000000000 ) ) ;
#7491 = ORIENTED_EDGE ( 'NONE', *, *, #2772, .F. ) ;
#7492 = VECTOR ( 'NONE', #8767, 1000.000000000000000 ) ;
#7493 = CARTESIAN_POINT ( 'NONE',  ( 48.49999999999995737, 90.00000000000000000, -10.00000000000000000 ) ) ;
#7494 = FACE_OUTER_BOUND ( 'NONE', #8520, .T. ) ;
#7495 = ORIENTED_EDGE ( 'NONE', *, *, #913, .F. ) ;
#7496 = SHAPE_REPRESENTATION_RELATIONSHIP ( 'NONE' , 'NONE' ,  #9937, #10604 ) ;
#7497 =( BOUNDED_CURVE ( )  B_SPLINE_CURVE ( 2, ( #1626, #10278, #763, #7766, #6589, #10711, #1557 ),
 .UNSPECIFIED., .F., .F. ) 
 B_SPLINE_CURVE_WITH_KNOTS ( ( 3, 2, 2, 3 ),
 ( 0.1999999999999999833, 0.2333333333333333925, 0.2666666666666668295, 0.3000000000000002109 ),
 .UNSPECIFIED. ) 
 CURVE ( )  GEOMETRIC_REPRESENTATION_ITEM ( )  RATIONAL_B_SPLINE_CURVE ( ( 1.000000000000000222, 0.8660254037844385966, 1.000000000000000000, 0.8660254037844387076, 1.000000000000000000, 0.8660254037844378194, 1.000000000000000888 ) ) 
 REPRESENTATION_ITEM ( '' )  );
#7498 = DIRECTION ( 'NONE',  ( 0.000000000000000000, 0.000000000000000000, 1.000000000000000000 ) ) ;
#7499 = CARTESIAN_POINT ( 'NONE',  ( 66.19999999999998863, 90.00000000000000000, 4.437500001229033764 ) ) ;
#7500 = EDGE_CURVE ( 'NONE', #3935, #6325, #11351, .T. ) ;
#7501 = DIRECTION ( 'NONE',  ( -1.000000000000000000, 0.000000000000000000, 0.000000000000000000 ) ) ;
#7502 = ORIENTED_EDGE ( 'NONE', *, *, #2802, .F. ) ;
#7503 = LINE ( 'NONE', #8678, #11599 ) ;
#7504 = LINE ( 'NONE', #10446, #2519 ) ;
#7505 = ORIENTED_EDGE ( 'NONE', *, *, #7925, .F. ) ;
#7506 = LINE ( 'NONE', #8992, #12249 ) ;
#7507 = ORIENTED_EDGE ( 'NONE', *, *, #5500, .F. ) ;
#7508 = AXIS2_PLACEMENT_3D ( 'NONE', #10098, #9119, #4290 ) ;
#7509 = CARTESIAN_POINT ( 'NONE',  ( 3.800000000000015365, 90.00000000000000000, 2.862500001229034474 ) ) ;
#7510 = VERTEX_POINT ( 'NONE', #4301 ) ;
#7511 = EDGE_CURVE ( 'NONE', #12815, #4991, #7815, .T. ) ;
#7512 = CARTESIAN_POINT ( 'NONE',  ( 1.040000000000000036, 0.5773502691896262862, -1.000000000000000000 ) ) ;
#7513 = CARTESIAN_POINT ( 'NONE',  ( 65.19999999999998863, 90.00000000000000000, 5.000000000000000000 ) ) ;
#7514 = APPLICATION_CONTEXT ( 'automotive_design' ) ;
#7515 = VERTEX_POINT ( 'NONE', #6187 ) ;
#7516 = PRODUCT_DEFINITION_SHAPE ( 'NONE', 'NONE',  #10725 ) ;
#7517 = VERTEX_POINT ( 'NONE', #8290 ) ;
#7519 = LINE ( 'NONE', #9286, #5114 ) ;
#7518 = AXIS2_PLACEMENT_3D ( 'NONE', #2252, #11260, #5248 ) ;
#7520 = ORIENTED_EDGE ( 'NONE', *, *, #2366, .F. ) ;
#7521 = EDGE_CURVE ( 'NONE', #4728, #6066, #2813, .T. ) ;
#7522 = CARTESIAN_POINT ( 'NONE',  ( -60.00000000000000000, -6.000000000000000000, 14.99999999999999645 ) ) ;
#7523 = CONTEXT_DEPENDENT_SHAPE_REPRESENTATION ( #4268, #1147 ) ;
#7524 = CARTESIAN_POINT ( 'NONE',  ( 35.00000000000000000, 126.0266567974326222, 3.650000001229034119 ) ) ;
#7525 = ORIENTED_EDGE ( 'NONE', *, *, #1360, .F. ) ;
#7526 =( LENGTH_UNIT ( ) NAMED_UNIT ( * ) SI_UNIT ( .MILLI., .METRE. ) );
#7527 = ORIENTED_EDGE ( 'NONE', *, *, #12466, .T. ) ;
#7528 = CARTESIAN_POINT ( 'NONE',  ( 5.000000000000004441, 27.00000000000000000, -2.500000000000000000 ) ) ;
#7529 = VERTEX_POINT ( 'NONE', #12278 ) ;
#7530 = EDGE_CURVE ( 'NONE', #7660, #5295, #12212, .T. ) ;
#7531 = CARTESIAN_POINT ( 'NONE',  ( 3.939444093506661027, 85.09162761845308864, 3.000000000000000444 ) ) ;
#7532 = CARTESIAN_POINT ( 'NONE',  ( 20.00000000000000355, 121.2009999999999934, -1.499999999999999556 ) ) ;
#7533 = ORIENTED_EDGE ( 'NONE', *, *, #1393, .F. ) ;
#7534 = ORIENTED_EDGE ( 'NONE', *, *, #9842, .T. ) ;
#7535 = CARTESIAN_POINT ( 'NONE',  ( 32.09707732552327286, 88.32801317409231956, -3.000000000000000000 ) ) ;
#7536 = ORIENTED_EDGE ( 'NONE', *, *, #7722, .T. ) ;
#7537 = VECTOR ( 'NONE', #6180, 1000.000000000000000 ) ;
#7538 = CARTESIAN_POINT ( 'NONE',  ( 66.44356964374998142, 108.1539533981018053, 3.771875000614516971 ) ) ;
#7539 = ORIENTED_EDGE ( 'NONE', *, *, #632, .F. ) ;
#7540 = CYLINDRICAL_SURFACE ( 'NONE', #2753, 6.499999999999999112 ) ;
#7541 = CARTESIAN_POINT ( 'NONE',  ( 30.00000000000000711, 0.000000000000000000, 10.00000000000000000 ) ) ;
#7542 = PLANE ( 'NONE',  #871 ) ;
#7543 = FACE_OUTER_BOUND ( 'NONE', #3383, .T. ) ;
#7544 = FACE_OUTER_BOUND ( 'NONE', #9614, .T. ) ;
#7545 = AXIS2_PLACEMENT_3D ( 'NONE', #6164, #1454, #6294 ) ;
#7546 = DIRECTION ( 'NONE',  ( -0.000000000000000000, 0.000000000000000000, -1.000000000000000000 ) ) ;
#7547 = EDGE_CURVE ( 'NONE', #8908, #12207, #10307, .T. ) ;
#7548 = LINE ( 'NONE', #11534, #3247 ) ;
#7549 = DIRECTION ( 'NONE',  ( 0.5877852522924715828, 0.8090169943749485615, 0.000000000000000000 ) ) ;
#7550 = CYLINDRICAL_SURFACE ( 'NONE', #1769, 3.349999999999995204 ) ;
#7551 = DIRECTION ( 'NONE',  ( -0.000000000000000000, 1.000000000000000000, -0.000000000000000000 ) ) ;
#7552 = VECTOR ( 'NONE', #12898, 1000.000000000000000 ) ;
#7553 = CARTESIAN_POINT ( 'NONE',  ( -23.49999999999999289, 51.07328482542158810, 3.000000000000000000 ) ) ;
#7554 = DIRECTION ( 'NONE',  ( 0.000000000000000000, 0.000000000000000000, -1.000000000000000000 ) ) ;
#7555 = EDGE_LOOP ( 'NONE', ( #12890, #7372, #2021, #9841 ) ) ;
#7556 = CYLINDRICAL_SURFACE ( 'NONE', #4847, 4.000000000000003553 ) ;
#7557 = CARTESIAN_POINT ( 'NONE',  ( 35.00000000000000000, 90.00000000000000000, -3.000000000000000888 ) ) ;
#7558 = EDGE_LOOP ( 'NONE', ( #5687, #7688, #6521, #5761 ) ) ;
#7559 = ADVANCED_FACE ( 'NONE', ( #6572 ), #9285, .F. ) ;
#7560 = SURFACE_STYLE_USAGE ( .BOTH. , #3579 ) ;
#7561 = ADVANCED_FACE ( 'NONE', ( #6638 ), #11417, .T. ) ;
#7562 = LINE ( 'NONE', #8550, #12413 ) ;
#7563 = DIRECTION ( 'NONE',  ( -0.000000000000000000, -0.000000000000000000, -1.000000000000000000 ) ) ;
#7564 = DIRECTION ( 'NONE',  ( -0.000000000000000000, 1.000000000000000000, -0.000000000000000000 ) ) ;
#7565 = ORIENTED_EDGE ( 'NONE', *, *, #4715, .T. ) ;
#7566 = CARTESIAN_POINT ( 'NONE',  ( -6.666666666666660745, 0.000000000000000000, 0.000000000000000000 ) ) ;
#7567 = CARTESIAN_POINT ( 'NONE',  ( 33.50000000000000711, 79.80000000000001137, 8.000000000000000000 ) ) ;
#7568 = ORIENTED_EDGE ( 'NONE', *, *, #10389, .F. ) ;
#7569 = DIRECTION ( 'NONE',  ( -0.000000000000000000, -0.000000000000000000, -1.000000000000000000 ) ) ;
#7570 = DIRECTION ( 'NONE',  ( 0.000000000000000000, -0.000000000000000000, 1.000000000000000000 ) ) ;
#7571 = EDGE_LOOP ( 'NONE', ( #3470, #12143 ) ) ;
#7572 = CIRCLE ( 'NONE', #7356, 1.424999999999999822 ) ;
#7573 = CARTESIAN_POINT ( 'NONE',  ( 25.00000000000000355, 0.000000000000000000, -7.349999999999996980 ) ) ;
#7574 = ORIENTED_EDGE ( 'NONE', *, *, #8672, .T. ) ;
#7575 = ADVANCED_FACE ( 'NONE', ( #10441 ), #12401, .F. ) ;
#7576 = CARTESIAN_POINT ( 'NONE',  ( 0.000000000000000000, -0.5773502691896253980, -1.000000000000000000 ) ) ;
#7577 = DIRECTION ( 'NONE',  ( -0.000000000000000000, -1.000000000000000000, -0.000000000000000000 ) ) ;
#7578 = DIRECTION ( 'NONE',  ( -1.000000000000000000, 0.000000000000000000, 0.000000000000000000 ) ) ;
#7579 = ORIENTED_EDGE ( 'NONE', *, *, #3992, .F. ) ;
#7580 = VECTOR ( 'NONE', #6523, 1000.000000000000000 ) ;
#7581 = FACE_OUTER_BOUND ( 'NONE', #8745, .T. ) ;
#7582 = VERTEX_POINT ( 'NONE', #11549 ) ;
#7583 = CARTESIAN_POINT ( 'NONE',  ( 31.50000000000000000, 90.00000000000000000, 4.000000000000000000 ) ) ;
#7584 = APPLICATION_PROTOCOL_DEFINITION ( 'draft international standard', 'automotive_design', 1998, #2267 ) ;
#7585 = CARTESIAN_POINT ( 'NONE',  ( 3.800000000000025135, 71.98667160128366049, 2.900000001229034563 ) ) ;
#7586 = ORIENTED_EDGE ( 'NONE', *, *, #2455, .T. ) ;
#7587 = ORIENTED_EDGE ( 'NONE', *, *, #2143, .F. ) ;
#7588 = DIRECTION ( 'NONE',  ( 1.000000000000000000, 0.000000000000000000, 0.000000000000000000 ) ) ;
#7589 = VERTEX_POINT ( 'NONE', #6702 ) ;
#7590 = EDGE_CURVE ( 'NONE', #6792, #4463, #8416, .T. ) ;
#7591 = CARTESIAN_POINT ( 'NONE',  ( 6.084625604134796362, 77.72058018632206711, 2.999999999999999556 ) ) ;
#7592 = COLOUR_RGB ( '',0.8941176470588234615, 0.8941176470588234615, 0.8941176470588234615 ) ;
#7593 = LINE ( 'NONE', #515, #11447 ) ;
#7594 = VECTOR ( 'NONE', #7986, 1000.000000000000000 ) ;
#7595 = VERTEX_POINT ( 'NONE', #2533 ) ;
#7596 = CARTESIAN_POINT ( 'NONE',  ( 50.72178482187499071, 117.2309300971526937, 2.909375000614517148 ) ) ;
#7597 = VERTEX_POINT ( 'NONE', #2663 ) ;
#7598 = EDGE_CURVE ( 'NONE', #1482, #2334, #7562, .T. ) ;
#7599 = FACE_OUTER_BOUND ( 'NONE', #12667, .T. ) ;
#7600 = EDGE_CURVE ( 'NONE', #307, #5827, #9526, .T. ) ;
#7601 = VERTEX_POINT ( 'NONE', #2594 ) ;
#7602 = CARTESIAN_POINT ( 'NONE',  ( 3.556430356250015024, 90.00000000000000000, 4.409375000614517148 ) ) ;
#7603 = ORIENTED_EDGE ( 'NONE', *, *, #4062, .F. ) ;
#7604 = FACE_OUTER_BOUND ( 'NONE', #8887, .T. ) ;
#7605 = AXIS2_PLACEMENT_3D ( 'NONE', #11758, #5991, #12805 ) ;
#7606 = DIRECTION ( 'NONE',  ( 0.000000000000000000, 0.000000000000000000, 1.000000000000000000 ) ) ;
#7607 = CARTESIAN_POINT ( 'NONE',  ( 5.000000000000004441, 30.00000000000000000, -10.00000000000000000 ) ) ;
#7608 = LINE ( 'NONE', #8596, #3311 ) ;
#7609 = PRODUCT_DEFINITION_FORMATION_WITH_SPECIFIED_SOURCE ( 'ANY', '', #4379, .NOT_KNOWN. ) ;
#7610 = DIRECTION ( 'NONE',  ( 0.000000000000000000, 0.000000000000000000, 1.000000000000000000 ) ) ;
#7611 = CARTESIAN_POINT ( 'NONE',  ( 1.649999999999999023, 0.000000000000000000, 0.000000000000000000 ) ) ;
#7612 = VECTOR ( 'NONE', #7486, 1000.000000000000227 ) ;
#7613 = DIRECTION ( 'NONE',  ( 0.000000000000000000, 0.000000000000000000, 1.000000000000000000 ) ) ;
#7614 = CARTESIAN_POINT ( 'NONE',  ( 3.678215178125014972, 90.00000000000000000, 4.732812500921776078 ) ) ;
#7615 = VECTOR ( 'NONE', #679, 1000.000000000000114 ) ;
#7616 = CARTESIAN_POINT ( 'NONE',  ( 0.000000000000000000, 0.000000000000000000, 0.000000000000000000 ) ) ;
#7617 = DIRECTION ( 'NONE',  ( -1.000000000000000000, 0.000000000000000000, 0.000000000000000000 ) ) ;
#7618 = CARTESIAN_POINT ( 'NONE',  ( 5.000000000000004441, 67.52776749732610995, 2.500000000000000444 ) ) ;
#7619 = EDGE_CURVE ( 'NONE', #237, #9364, #6443, .T. ) ;
#7620 = EDGE_LOOP ( 'NONE', ( #642, #12614, #842, #4058 ) ) ;
#7621 = CARTESIAN_POINT ( 'NONE',  ( 6.499999999999997335, 65.10243346208218895, -1.000000000000000888 ) ) ;
#7622 = LINE ( 'NONE', #12666, #12276 ) ;
#7623 = EDGE_LOOP ( 'NONE', ( #10669, #4504, #9752, #5812 ) ) ;
#7624 = VECTOR ( 'NONE', #6818, 1000.000000000000000 ) ;
#7625 = VECTOR ( 'NONE', #6623, 1000.000000000000000 ) ;
#7626 = DIRECTION ( 'NONE',  ( 0.000000000000000000, 0.000000000000000000, 1.000000000000000000 ) ) ;
#7627 = DIRECTION ( 'NONE',  ( 1.000000000000000000, 0.000000000000000000, -0.000000000000000000 ) ) ;
#7628 = ORIENTED_EDGE ( 'NONE', *, *, #8358, .T. ) ;
#7629 = EDGE_CURVE ( 'NONE', #12180, #12399, #3516, .T. ) ;
#7630 = DIRECTION ( 'NONE',  ( 0.5000000000000036637, -0.8660254037844365982, 0.000000000000000000 ) ) ;
#7631 = CARTESIAN_POINT ( 'NONE',  ( 66.44356964374999563, 90.00000000000000000, 4.128125000614517148 ) ) ;
#7632 = VECTOR ( 'NONE', #1562, 1000.000000000000000 ) ;
#7633 = CARTESIAN_POINT ( 'NONE',  ( 1.040000000000000036, -1.154700538379251240, 1.014316938424154191E-17 ) ) ;
#7634 = LINE ( 'NONE', #2477, #533 ) ;
#7635 = EDGE_CURVE ( 'NONE', #7791, #4025, #7408, .T. ) ;
#7636 = ORIENTED_EDGE ( 'NONE', *, *, #2916, .F. ) ;
#7637 = DIRECTION ( 'NONE',  ( -0.000000000000000000, -0.000000000000000000, -1.000000000000000000 ) ) ;
#7638 = VERTEX_POINT ( 'NONE', #7432 ) ;
#7639 = DIRECTION ( 'NONE',  ( 0.1305261922200528224, 0.9914448613738103822, -0.000000000000000000 ) ) ;
#7640 = LINE ( 'NONE', #9666, #2485 ) ;
#7641 = VECTOR ( 'NONE', #8866, 1000.000000000000000 ) ;
#7642 = CIRCLE ( 'NONE', #10139, 2.849999999999999645 ) ;
#7643 = DIRECTION ( 'NONE',  ( -1.000000000000000000, 0.000000000000000000, 0.000000000000000000 ) ) ;
#7644 = CARTESIAN_POINT ( 'NONE',  ( 45.00000000000000000, -5.000000000000000000, -7.250000000000000888 ) ) ;
#7645 = CARTESIAN_POINT ( 'NONE',  ( -56.05384757729341061, 33.16506350946112036, 0.000000000000000000 ) ) ;
#7646 = ORIENTED_EDGE ( 'NONE', *, *, #7435, .T. ) ;
#7647 = DIRECTION ( 'NONE',  ( 0.000000000000000000, 1.000000000000000000, 0.000000000000000000 ) ) ;
#7648 = ITEM_DEFINED_TRANSFORMATION ( 'NONE', 'NONE', #4887,  #5704 ) ;
#7649 = LINE ( 'NONE', #2877, #11901 ) ;
#7650 = ADVANCED_FACE ( 'NONE', ( #8675 ), #9455, .T. ) ;
#7651 = ORIENTED_EDGE ( 'NONE', *, *, #9484, .T. ) ;
#7652 = CIRCLE ( 'NONE', #12246, 30.00000000000000000 ) ;
#7653 = CARTESIAN_POINT ( 'NONE',  ( 45.00000000000000000, 0.000000000000000000, 4.249999999999999112 ) ) ;
#7654 = ORIENTED_EDGE ( 'NONE', *, *, #12761, .F. ) ;
#7655 = AXIS2_PLACEMENT_3D ( 'NONE', #425, #8682, #1549 ) ;
#7656 = SURFACE_SIDE_STYLE ('',( #12631 ) ) ;
#7657 = ORIENTED_EDGE ( 'NONE', *, *, #9788, .F. ) ;
#7658 = DIRECTION ( 'NONE',  ( -1.000000000000000000, 0.000000000000000000, 0.000000000000000000 ) ) ;
#7659 = UNCERTAINTY_MEASURE_WITH_UNIT (LENGTH_MEASURE( 1.000000000000000082E-05 ), #2044, 'distance_accuracy_value', 'NONE');
#7660 = VERTEX_POINT ( 'NONE', #2468 ) ;
#7661 = AXIS2_PLACEMENT_3D ( 'NONE', #2381, #3369, #7606 ) ;
#7662 = LINE ( 'NONE', #1709, #9720 ) ;
#7663 = VERTEX_POINT ( 'NONE', #3709 ) ;
#7664 = CARTESIAN_POINT ( 'NONE',  ( 3.800000000000015365, 90.00000000000000000, 2.862500001229034474 ) ) ;
#7665 = EDGE_CURVE ( 'NONE', #1779, #11619, #12539, .T. ) ;
#7666 = EDGE_LOOP ( 'NONE', ( #7824, #8899, #1424, #12224 ) ) ;
#7667 = CARTESIAN_POINT ( 'NONE',  ( 35.00000000000000711, 53.69209320379640360, 4.465625000614517504 ) ) ;
#7668 = VERTEX_POINT ( 'NONE', #10503 ) ;
#7669 = DIRECTION ( 'NONE',  ( -1.000000000000000000, 0.000000000000000000, 1.301042606982605321E-15 ) ) ;
#7670 = CARTESIAN_POINT ( 'NONE',  ( 3.799999999999985612, 108.0133283987162827, 4.062500000000000000 ) ) ;
#7671 = CONICAL_SURFACE ( 'NONE', #6207, 1.499999999999999556, 1.029744260000000189 ) ;
#7672 = FACE_OUTER_BOUND ( 'NONE', #1143, .T. ) ;
#7673 = CARTESIAN_POINT ( 'NONE',  ( 3.556430356250014579, 108.1539533981018053, 2.965625000614517504 ) ) ;
#7674 = EDGE_CURVE ( 'NONE', #5477, #11221, #8241, .T. ) ;
#7675 = EDGE_CURVE ( 'NONE', #12353, #10525, #10574, .T. ) ;
#7676 = DIRECTION ( 'NONE',  ( 1.000000000000000000, 0.000000000000000000, 1.084202172485503571E-16 ) ) ;
#7677 = CARTESIAN_POINT ( 'NONE',  ( 3.800000000000055334, 71.98667160128364628, 3.800000001229034474 ) ) ;
#7678 = CARTESIAN_POINT ( 'NONE',  ( -61.13397459621555186, 31.96410161513774284, 0.000000000000000000 ) ) ;
#7679 = CARTESIAN_POINT ( 'NONE',  ( 63.68224097532933570, 98.79369391286385849, -0.9999999999999970024 ) ) ;
#7680 = VECTOR ( 'NONE', #1734, 999.9999999999998863 ) ;
#7681 = EDGE_CURVE ( 'NONE', #4333, #992, #3581, .T. ) ;
#7682 = DIRECTION ( 'NONE',  ( 1.000000000000000000, 0.000000000000000000, 0.000000000000000000 ) ) ;
#7683 = APPLICATION_CONTEXT ( 'automotive_design' ) ;
#7684 = LINE ( 'NONE', #12722, #847 ) ;
#7685 = CARTESIAN_POINT ( 'NONE',  ( 3.556430356250028790, 71.84604660189818048, 3.546875000614516882 ) ) ;
#7686 = VERTEX_POINT ( 'NONE', #10696 ) ;
#7687 = CARTESIAN_POINT ( 'NONE',  ( 1.749999999999999112, 0.000000000000000000, 0.000000000000000000 ) ) ;
#7688 = ORIENTED_EDGE ( 'NONE', *, *, #2653, .T. ) ;
#7689 =( NAMED_UNIT ( * ) PLANE_ANGLE_UNIT ( ) SI_UNIT ( $, .RADIAN. ) );
#7690 = EDGE_CURVE ( 'NONE', #5204, #12162, #8612, .T. ) ;
#7691 = CARTESIAN_POINT ( 'NONE',  ( 0.000000000000000000, 0.4117131682837005258, 0.000000000000000000 ) ) ;
#7692 = EDGE_CURVE ( 'NONE', #2762, #9176, #9715, .T. ) ;
#7693 = CARTESIAN_POINT ( 'NONE',  ( 12.55092940903992194, 109.9007343985615393, -0.9999999999999970024 ) ) ;
#7694 = CARTESIAN_POINT ( 'NONE',  ( -60.00000000000000000, 0.000000000000000000, -15.00000000000000355 ) ) ;
#7695 = VECTOR ( 'NONE', #5208, 1000.000000000000000 ) ;
#7696 = FACE_OUTER_BOUND ( 'NONE', #8456, .T. ) ;
#7697 = VECTOR ( 'NONE', #2417, 1000.000000000000227 ) ;
#7698 = CARTESIAN_POINT ( 'NONE',  ( 20.00000000000000355, 0.000000000000000000, -1.499999999999999556 ) ) ;
#7699 = CARTESIAN_POINT ( 'NONE',  ( -53.33333333333332149, 79.07477288111861924, -1.000000000000000000 ) ) ;
#7700 = EDGE_LOOP ( 'NONE', ( #8441, #12251, #10579, #2530 ) ) ;
#7701 = LINE ( 'NONE', #2479, #10598 ) ;
#7702 = VERTEX_POINT ( 'NONE', #1998 ) ;
#7703 = CARTESIAN_POINT ( 'NONE',  ( 3.800000000000015365, 90.00000000000000000, 3.762500001229034385 ) ) ;
#7704 = DIRECTION ( 'NONE',  ( 0.000000000000000000, 0.000000000000000000, 1.000000000000000000 ) ) ;
#7705 = ADVANCED_FACE ( 'NONE', ( #7816 ), #6042, .F. ) ;
#7706 = AXIS2_PLACEMENT_3D ( 'NONE', #2676, #3596, #3045 ) ;
#7707 = DIRECTION ( 'NONE',  ( -1.000000000000000000, 0.000000000000000000, 0.000000000000000000 ) ) ;
#7708 = ADVANCED_FACE ( 'NONE', ( #3903 ), #872, .F. ) ;
#7709 = ORIENTED_EDGE ( 'NONE', *, *, #9615, .T. ) ;
#7710 = DIRECTION ( 'NONE',  ( -1.000000000000000000, 0.000000000000000000, 0.000000000000000000 ) ) ;
#7711 = ORIENTED_EDGE ( 'NONE', *, *, #1595, .T. ) ;
#7712 = DIRECTION ( 'NONE',  ( -1.000000000000000000, 0.000000000000000000, 0.000000000000000000 ) ) ;
#7713 = CARTESIAN_POINT ( 'NONE',  ( 1.040000000000000036, -0.8660254037844384856, -0.5000000000000003331 ) ) ;
#7714 = ORIENTED_EDGE ( 'NONE', *, *, #7034, .F. ) ;
#7715 = CIRCLE ( 'NONE', #9804, 1.499999999999999556 ) ;
#7716 = ORIENTED_EDGE ( 'NONE', *, *, #1875, .T. ) ;
#7717 = CIRCLE ( 'NONE', #3125, 2.849999999999999645 ) ;
#7718 = CARTESIAN_POINT ( 'NONE',  ( 3.068288344391240763, -2.655262421758693314, -0.8000000000000000444 ) ) ;
#7719 = ORIENTED_EDGE ( 'NONE', *, *, #11408, .T. ) ;
#7720 = CARTESIAN_POINT ( 'NONE',  ( 7.795990775014339569, 74.32053629685827900, 3.000000000000002665 ) ) ;
#7721 = CARTESIAN_POINT ( 'NONE',  ( 35.00000000000000000, 90.00000000000000000, -3.799999999999999822 ) ) ;
#7722 = EDGE_CURVE ( 'NONE', #6839, #11292, #7885, .T. ) ;
#7723 = AXIS2_PLACEMENT_3D ( 'NONE', #3808, #4001, #9876 ) ;
#7724 = EDGE_CURVE ( 'NONE', #5204, #11636, #8799, .T. ) ;
#7725 = ORIENTED_EDGE ( 'NONE', *, *, #9057, .F. ) ;
#7726 = LINE ( 'NONE', #5944, #12437 ) ;
#7727 = VERTEX_POINT ( 'NONE', #5001 ) ;
#7728 = CARTESIAN_POINT ( 'NONE',  ( 0.000000000000000000, 0.000000000000000000, 0.000000000000000000 ) ) ;
#7729 = ORIENTED_EDGE ( 'NONE', *, *, #9817, .F. ) ;
#7730 = CARTESIAN_POINT ( 'NONE',  ( 3.556430356250014579, 108.1539533981018053, 2.965625000614517504 ) ) ;
#7731 = VERTEX_POINT ( 'NONE', #12000 ) ;
#7732 = CIRCLE ( 'NONE', #9399, 2.849999999999999201 ) ;
#7733 = CARTESIAN_POINT ( 'NONE',  ( 35.00000000000000000, 90.00000000000000000, 22.38477631085024555 ) ) ;
#7734 = CARTESIAN_POINT ( 'NONE',  ( 3.350000000000000089, 0.000000000000000000, 0.000000000000000000 ) ) ;
#7735 = FACE_OUTER_BOUND ( 'NONE', #6029, .T. ) ;
#7736 = CARTESIAN_POINT ( 'NONE',  ( 19.27821517812503060, 62.76906990284727783, 3.528125000614517059 ) ) ;
#7737 = EDGE_CURVE ( 'NONE', #12915, #1292, #11934, .T. ) ;
#7738 = DIRECTION ( 'NONE',  ( -1.000000000000000000, 0.000000000000000000, 0.000000000000000000 ) ) ;
#7739 = VECTOR ( 'NONE', #5794, 1000.000000000000114 ) ;
#7740 = FACE_OUTER_BOUND ( 'NONE', #11068, .T. ) ;
#7741 = AXIS2_PLACEMENT_3D ( 'NONE', #1203, #9379, #2328 ) ;
#7742 = CARTESIAN_POINT ( 'NONE',  ( -65.00000000000004263, 38.66025403784436065, -3.000000000000000000 ) ) ;
#7743 = CARTESIAN_POINT ( 'NONE',  ( 25.68387172342410807, 120.0032449382199928, 2.999999999999998224 ) ) ;
#7744 = CYLINDRICAL_SURFACE ( 'NONE', #948, 31.19999999999998863 ) ;
#7745 = DIRECTION ( 'NONE',  ( 8.673617379884034486E-16, 5.007715329123921945E-16, -1.000000000000000000 ) ) ;
#7746 = CARTESIAN_POINT ( 'NONE',  ( 50.72178482187499071, 117.2309300971526937, 3.359375000614517326 ) ) ;
#7747 = ORIENTED_EDGE ( 'NONE', *, *, #9329, .F. ) ;
#7748 = CARTESIAN_POINT ( 'NONE',  ( 66.20000000000000284, 71.98667160128370313, 3.387500000000000178 ) ) ;
#7749 = CIRCLE ( 'NONE', #11291, 28.99999999999999289 ) ;
#7750 = DIRECTION ( 'NONE',  ( -0.000000000000000000, -0.000000000000000000, -1.000000000000000000 ) ) ;
#7751 = ORIENTED_EDGE ( 'NONE', *, *, #5381, .F. ) ;
#7752 = CARTESIAN_POINT ( 'NONE',  ( 25.00000000000000355, -5.000000000000000000, -5.750000000000000000 ) ) ;
#7753 = DIRECTION ( 'NONE',  ( 0.000000000000000000, 0.000000000000000000, 1.000000000000000000 ) ) ;
#7754 = VECTOR ( 'NONE', #10552, 1000.000000000000000 ) ;
#7755 = DIRECTION ( 'NONE',  ( 0.000000000000000000, 0.000000000000000000, -1.000000000000000000 ) ) ;
#7756 = ADVANCED_FACE ( 'NONE', ( #9971 ), #1804, .T. ) ;
#7757 = CARTESIAN_POINT ( 'NONE',  ( 19.27821517812503060, 62.76906990284727783, 3.078125000614517326 ) ) ;
#7758 = EDGE_CURVE ( 'NONE', #11518, #12039, #2063, .T. ) ;
#7759 = DIRECTION ( 'NONE',  ( -0.000000000000000000, 1.000000000000000000, -0.000000000000000000 ) ) ;
#7760 = CARTESIAN_POINT ( 'NONE',  ( 66.44356964375000985, 71.84604660189820891, 4.596875000614516260 ) ) ;
#7761 = ORIENTED_EDGE ( 'NONE', *, *, #10496, .F. ) ;
#7762 = DIRECTION ( 'NONE',  ( 0.8958148394926558344, 0.4444274669107966536, 4.977592430910269431E-17 ) ) ;
#7763 = ORIENTED_EDGE ( 'NONE', *, *, #6757, .F. ) ;
#7764 =( GEOMETRIC_REPRESENTATION_CONTEXT ( 3 ) GLOBAL_UNCERTAINTY_ASSIGNED_CONTEXT ( ( #6190 ) ) GLOBAL_UNIT_ASSIGNED_CONTEXT ( ( #7461, #3610, #3990 ) ) REPRESENTATION_CONTEXT ( 'NONE', 'WORKASPACE' ) );
#7765 = FACE_OUTER_BOUND ( 'NONE', #2851, .T. ) ;
#7766 = CARTESIAN_POINT ( 'NONE',  ( 35.00000000000000000, 126.0266567974326222, 4.437500000000000888 ) ) ;
#7767 = LINE ( 'NONE', #3980, #690 ) ;
#7768 = DIRECTION ( 'NONE',  ( -0.5877852522924715828, -0.8090169943749484505, 0.000000000000000000 ) ) ;
#7769 = CARTESIAN_POINT ( 'NONE',  ( -60.00000000000000000, 0.000000000000000000, 14.99999999999999645 ) ) ;
#7770 = ORIENTED_EDGE ( 'NONE', *, *, #9281, .F. ) ;
#7771 = FACE_OUTER_BOUND ( 'NONE', #7255, .T. ) ;
#7772 = CARTESIAN_POINT ( 'NONE',  ( -3.350000000000000089, 4.102566777143633281E-16, 0.000000000000000000 ) ) ;
#7773 = ORIENTED_EDGE ( 'NONE', *, *, #1503, .F. ) ;
#7774 = PRESENTATION_LAYER_ASSIGNMENT (  '', '', ( #8407 ) ) ;
#7775 = FILL_AREA_STYLE_COLOUR ( '', #949 ) ;
#7776 = ORIENTED_EDGE ( 'NONE', *, *, #756, .F. ) ;
#7777 = B_SPLINE_CURVE_WITH_KNOTS ( 'NONE', 3,
 ( #12009, #10044, #12741, #2928 ),
 .UNSPECIFIED., .F., .F.,
 ( 4, 4 ),
 ( 0.000000000000000000, 1.000000000000000000 ),
 .UNSPECIFIED. ) ;
#7778 = DIRECTION ( 'NONE',  ( -0.8660254037844361541, -0.5000000000000042188, 0.000000000000000000 ) ) ;
#7779 = ORIENTED_EDGE ( 'NONE', *, *, #4324, .F. ) ;
#7780 = EDGE_CURVE ( 'NONE', #4305, #8971, #5910, .T. ) ;
#7781 = CARTESIAN_POINT ( 'NONE',  ( 11.55549086838933981, 69.15209071451751299, 3.000000000000000444 ) ) ;
#7782 = PLANE ( 'NONE',  #3738 ) ;
#7783 = CIRCLE ( 'NONE', #12176, 1.500000000000001332 ) ;
#7784 = ORIENTED_EDGE ( 'NONE', *, *, #9147, .T. ) ;
#7785 = DIRECTION ( 'NONE',  ( 0.000000000000000000, 0.000000000000000000, -1.000000000000000000 ) ) ;
#7786 = VERTEX_POINT ( 'NONE', #6831 ) ;
#7787 = PLANE ( 'NONE',  #10015 ) ;
#7788 = ORIENTED_EDGE ( 'NONE', *, *, #300, .F. ) ;
#7789 = EDGE_CURVE ( 'NONE', #376, #6806, #3021, .T. ) ;
#7790 = CARTESIAN_POINT ( 'NONE',  ( 3.556430356250015024, 90.00000000000000000, 4.353125000614517681 ) ) ;
#7791 = VERTEX_POINT ( 'NONE', #1868 ) ;
#7792 = CARTESIAN_POINT ( 'NONE',  ( 20.00000000000000355, 2.000000000000000000, 10.00000000000000000 ) ) ;
#7793 = DIRECTION ( 'NONE',  ( 0.000000000000000000, 0.000000000000000000, 1.000000000000000000 ) ) ;
#7794 = EDGE_CURVE ( 'NONE', #12180, #8074, #12638, .T. ) ;
#7795 = CARTESIAN_POINT ( 'NONE',  ( 31.99902028769960438, 88.51116798584881451, -3.000000000000000000 ) ) ;
#7796 = CARTESIAN_POINT ( 'NONE',  ( 50.72178482187499071, 117.2309300971526937, 4.203125000614517326 ) ) ;
#7797 = AXIS2_PLACEMENT_3D ( 'NONE', #9154, #3087, #1174 ) ;
#7798 = FACE_OUTER_BOUND ( 'NONE', #1879, .T. ) ;
#7799 = CARTESIAN_POINT ( 'NONE',  ( 1.269999999999999796, 0.000000000000000000, 0.000000000000000000 ) ) ;
#7800 = CARTESIAN_POINT ( 'NONE',  ( 21.49999999999998579, 90.00000000000000000, -10.00000000000000000 ) ) ;
#7801 = DIRECTION ( 'NONE',  ( -0.000000000000000000, -0.000000000000000000, 1.000000000000000000 ) ) ;
#7802 = DIRECTION ( 'NONE',  ( 1.000000000000000000, 0.000000000000000000, -8.673617379884034486E-16 ) ) ;
#7803 = CLOSED_SHELL ( 'NONE', ( #7395, #3258, #11855, #3534, #5894, #7124, #9022, #6425, #8157, #7756, #10035, #7561, #11648, #482, #375, #4024, #10914, #11754, #11139, #2647, #12030, #9773, #7575 ) ) ;
#7804 = DIRECTION ( 'NONE',  ( 1.000000000000000000, 0.000000000000000000, 0.000000000000000000 ) ) ;
#7805 = ORIENTED_EDGE ( 'NONE', *, *, #5640, .F. ) ;
#7806 = EDGE_CURVE ( 'NONE', #3174, #11441, #4478, .T. ) ;
#7807 = LINE ( 'NONE', #4615, #2954 ) ;
#7808 = CARTESIAN_POINT ( 'NONE',  ( 66.44356964374998142, 108.1539533981018053, 4.671875000614516438 ) ) ;
#7809 = ORIENTED_EDGE ( 'NONE', *, *, #12064, .F. ) ;
#7811 = FACE_OUTER_BOUND ( 'NONE', #9215, .T. ) ;
#7810 = AXIS2_PLACEMENT_3D ( 'NONE', #6275, #8115, #7324 ) ;
#7812 = CARTESIAN_POINT ( 'NONE',  ( 3.799999999999985612, 108.0133283987162827, 3.725000001229034741 ) ) ;
#7813 = ORIENTED_EDGE ( 'NONE', *, *, #254, .T. ) ;
#7814 = AXIS2_PLACEMENT_3D ( 'NONE', #6625, #5585, #11471 ) ;
#7815 = CIRCLE ( 'NONE', #7190, 4.999999999999997335 ) ;
#7816 = FACE_OUTER_BOUND ( 'NONE', #9815, .T. ) ;
#7817 = DIRECTION ( 'NONE',  ( -1.000000000000000000, 0.000000000000000000, -0.000000000000000000 ) ) ;
#7818 = DIRECTION ( 'NONE',  ( -1.000000000000000000, 0.000000000000000000, 0.000000000000000000 ) ) ;
#7819 = CARTESIAN_POINT ( 'NONE',  ( 3.556430356250028790, 71.84604660189818048, 3.490625000614516971 ) ) ;
#7820 = ADVANCED_FACE ( 'NONE', ( #5852 ), #3047, .F. ) ;
#7821 = DIRECTION ( 'NONE',  ( -1.000000000000000000, 0.000000000000000000, 0.000000000000000000 ) ) ;
#7822 = AXIS2_PLACEMENT_3D ( 'NONE', #11798, #990, #4926 ) ;
#7823 = CARTESIAN_POINT ( 'NONE',  ( 0.000000000000000000, 0.5773502691896262862, -1.000000000000000000 ) ) ;
#7824 = ORIENTED_EDGE ( 'NONE', *, *, #2066, .F. ) ;
#7825 = VECTOR ( 'NONE', #9562, 1000.000000000000000 ) ;
#7826 = DIRECTION ( 'NONE',  ( -0.000000000000000000, -1.000000000000000000, -0.000000000000000000 ) ) ;
#7827 = ORIENTED_EDGE ( 'NONE', *, *, #10710, .T. ) ;
#7828 = CARTESIAN_POINT ( 'NONE',  ( 9.999999999999994671, 70.41451884327426569, 3.000000000000000000 ) ) ;
#7829 = ADVANCED_FACE ( 'NONE', ( #5790 ), #3773, .T. ) ;
#7830 = EDGE_CURVE ( 'NONE', #6548, #1939, #11741, .T. ) ;
#7831 = LINE ( 'NONE', #1079, #7066 ) ;
#7832 = LINE ( 'NONE', #1015, #12811 ) ;
#7833 = CIRCLE ( 'NONE', #4294, 4.999999999999997335 ) ;
#7834 = DIRECTION ( 'NONE',  ( -0.000000000000000000, 1.000000000000000000, -0.000000000000000000 ) ) ;
#7835 = CIRCLE ( 'NONE', #11809, 3.351416843938787249 ) ;
#7836 = CARTESIAN_POINT ( 'NONE',  ( 2.168404344971008868E-16, 0.000000000000000000, 0.000000000000000000 ) ) ;
#7837 = VERTEX_POINT ( 'NONE', #10762 ) ;
#7838 = FACE_OUTER_BOUND ( 'NONE', #8247, .T. ) ;
#7839 = DIRECTION ( 'NONE',  ( 0.000000000000000000, 0.000000000000000000, 1.000000000000000000 ) ) ;
#7840 = VERTEX_POINT ( 'NONE', #10884 ) ;
#7841 = FACE_OUTER_BOUND ( 'NONE', #10003, .T. ) ;
#7842 = ORIENTED_EDGE ( 'NONE', *, *, #6960, .F. ) ;
#7843 = CARTESIAN_POINT ( 'NONE',  ( 35.00000000000000000, 90.00000000000000000, 4.800000000000000711 ) ) ;
#7845 = ORIENTED_EDGE ( 'NONE', *, *, #6703, .F. ) ;
#7844 = VECTOR ( 'NONE', #1330, 1000.000000000000000 ) ;
#7846 = VECTOR ( 'NONE', #4049, 1000.000000000000000 ) ;
#7847 = DIRECTION ( 'NONE',  ( -1.000000000000000000, 0.000000000000000000, 0.000000000000000000 ) ) ;
#7848 = CARTESIAN_POINT ( 'NONE',  ( 35.00000000000000000, 90.00000000000000000, 4.000000000000000000 ) ) ;
#7849 = ORIENTED_EDGE ( 'NONE', *, *, #5067, .T. ) ;
#7850 = MANIFOLD_SOLID_BREP ( 'Extrude-Thin4', #6552 ) ;
#7851 = DIRECTION ( 'NONE',  ( -0.000000000000000000, 0.000000000000000000, -1.000000000000000000 ) ) ;
#7852 = ORIENTED_EDGE ( 'NONE', *, *, #6522, .F. ) ;
#7853 =( REPRESENTATION_RELATIONSHIP ('NONE','NONE', #1997, #2422 ) REPRESENTATION_RELATIONSHIP_WITH_TRANSFORMATION ( #6401 )SHAPE_REPRESENTATION_RELATIONSHIP( ) );
#7854 = EDGE_CURVE ( 'NONE', #4270, #11429, #4897, .T. ) ;
#7855 = DIRECTION ( 'NONE',  ( 0.000000000000000000, 0.000000000000000000, 1.000000000000000000 ) ) ;
#7856 = AXIS2_PLACEMENT_3D ( 'NONE', #8619, #2604, #8495 ) ;
#7857 = ORIENTED_EDGE ( 'NONE', *, *, #6031, .T. ) ;
#7858 = CARTESIAN_POINT ( 'NONE',  ( 50.72178482187501203, 62.76906990284730625, 3.153125000614517504 ) ) ;
#7859 = ORIENTED_EDGE ( 'NONE', *, *, #8275, .T. ) ;
#7860 = CARTESIAN_POINT ( 'NONE',  ( -54.07179676972453564, 35.73205080756889629, -1.000000000000000000 ) ) ;
#7861 = CARTESIAN_POINT ( 'NONE',  ( 3.800000000000015365, 90.00000000000000000, 3.200000000000000178 ) ) ;
#7862 = CARTESIAN_POINT ( 'NONE',  ( 50.60000000000001563, 62.98000740192552627, 3.462500001229034563 ) ) ;
#7863 = CARTESIAN_POINT ( 'NONE',  ( 35.00000000000000000, 126.3079067962035822, 2.890625000614516882 ) ) ;
#7864 = VECTOR ( 'NONE', #1602, 1000.000000000000000 ) ;
#7865 = EDGE_CURVE ( 'NONE', #10542, #2484, #11077, .T. ) ;
#7866 = DIRECTION ( 'NONE',  ( -0.8660254037844361541, -0.5000000000000042188, 0.000000000000000000 ) ) ;
#7867 = ORIENTED_EDGE ( 'NONE', *, *, #9188, .T. ) ;
#7868 = CARTESIAN_POINT ( 'NONE',  ( 19.40000000000000924, 117.0199925980744666, 4.924999999999999822 ) ) ;
#7869 = EDGE_CURVE ( 'NONE', #5747, #7529, #9317, .T. ) ;
#7870 = DIRECTION ( 'NONE',  ( 0.000000000000000000, 0.000000000000000000, 1.000000000000000000 ) ) ;
#7871 = LINE ( 'NONE', #9959, #5526 ) ;
#7872 = EDGE_LOOP ( 'NONE', ( #10732, #3233, #4586 ) ) ;
#7873 = CARTESIAN_POINT ( 'NONE',  ( 1.649999999999999911, 0.000000000000000000, 0.000000000000000000 ) ) ;
#7874 = EDGE_CURVE ( 'NONE', #8099, #4634, #11140, .T. ) ;
#7875 = VERTEX_POINT ( 'NONE', #140 ) ;
#7876 = VECTOR ( 'NONE', #347, 1000.000000000000000 ) ;
#7877 = FACE_OUTER_BOUND ( 'NONE', #7872, .T. ) ;
#7878 = CARTESIAN_POINT ( 'NONE',  ( 35.00000000000000711, 53.69209320379640360, 4.521875000614516971 ) ) ;
#7879 = ORIENTED_EDGE ( 'NONE', *, *, #831, .T. ) ;
#7880 = CARTESIAN_POINT ( 'NONE',  ( 66.44356964374998142, 108.1539533981018053, 3.771875000614516971 ) ) ;
#7881 = LINE ( 'NONE', #11933, #7680 ) ;
#7882 = ORIENTED_EDGE ( 'NONE', *, *, #7437, .T. ) ;
#7883 = ADVANCED_FACE ( 'NONE', ( #12196 ), #8080, .T. ) ;
#7884 = CIRCLE ( 'NONE', #3726, 1.500000000000001332 ) ;
#7885 = LINE ( 'NONE', #4874, #1123 ) ;
#7886 = EDGE_CURVE ( 'NONE', #362, #1479, #4288, .T. ) ;
#7887 = CARTESIAN_POINT ( 'NONE',  ( 20.00000000000000355, 2.000000000000000000, 10.00000000000000000 ) ) ;
#7888 = LINE ( 'NONE', #2981, #3685 ) ;
#7889 = LINE ( 'NONE', #2983, #9200 ) ;
#7890 = CYLINDRICAL_SURFACE ( 'NONE', #9750, 31.19999999999998863 ) ;
#7891 = ORIENTED_EDGE ( 'NONE', *, *, #6705, .F. ) ;
#7892 = AXIS2_PLACEMENT_3D ( 'NONE', #12063, #3110, #4089 ) ;
#7893 = DIRECTION ( 'NONE',  ( -0.000000000000000000, -0.000000000000000000, 1.000000000000000000 ) ) ;
#7894 = ORIENTED_EDGE ( 'NONE', *, *, #6127, .T. ) ;
#7895 = CARTESIAN_POINT ( 'NONE',  ( 6.499999999999999112, 79.07477288111861924, 0.9999999999999997780 ) ) ;
#7896 = ADVANCED_FACE ( 'NONE', ( #4349, #12328 ), #5060, .T. ) ;
#7897 = CARTESIAN_POINT ( 'NONE',  ( -48.33333333333332860, 0.000000000000000000, -1.500000000000003109 ) ) ;
#7898 = DIRECTION ( 'NONE',  ( -0.3090169943749500048, 0.9510565162951528650, 0.000000000000000000 ) ) ;
#7899 = AXIS2_PLACEMENT_3D ( 'NONE', #9545, #8321, #7707 ) ;
#7900 = LINE ( 'NONE', #6784, #11571 ) ;
#7901 = AXIS2_PLACEMENT_3D ( 'NONE', #397, #12587, #12324 ) ;
#7902 = DIRECTION ( 'NONE',  ( 0.000000000000000000, 0.000000000000000000, 1.000000000000000000 ) ) ;
#7903 = ADVANCED_FACE ( 'NONE', ( #269 ), #8340, .T. ) ;
#7904 = ORIENTED_EDGE ( 'NONE', *, *, #7272, .T. ) ;
#7905 = DIRECTION ( 'NONE',  ( 0.000000000000000000, 0.000000000000000000, -1.000000000000000000 ) ) ;
#7906 = CARTESIAN_POINT ( 'NONE',  ( -2.387319993259524598, -4.036502139894371233, -0.8000000000000000444 ) ) ;
#7907 = ORIENTED_EDGE ( 'NONE', *, *, #7722, .F. ) ;
#7908 = SURFACE_STYLE_FILL_AREA ( #3926 ) ;
#7909 = ORIENTED_EDGE ( 'NONE', *, *, #11341, .F. ) ;
#7910 = ADVANCED_FACE ( 'NONE', ( #12264 ), #78, .T. ) ;
#7911 = ORIENTED_EDGE ( 'NONE', *, *, #5254, .F. ) ;
#7912 = AXIS2_PLACEMENT_3D ( 'NONE', #821, #8012, #12682 ) ;
#7913 = CARTESIAN_POINT ( 'NONE',  ( 35.75000000000000711, 92.49999999999998579, -3.000000000000000000 ) ) ;
#7914 =( BOUNDED_CURVE ( )  B_SPLINE_CURVE ( 2, ( #7861, #4917, #1653, #3945, #2643, #2707, #5642 ),
 .UNSPECIFIED., .F., .F. ) 
 B_SPLINE_CURVE_WITH_KNOTS ( ( 3, 2, 2, 3 ),
 ( 0.8000000000000002665, 0.8333333333333334814, 0.8666666666666666963, 0.8887752022894196413 ),
 .UNSPECIFIED. ) 
 CURVE ( )  GEOMETRIC_REPRESENTATION_ITEM ( )  RATIONAL_B_SPLINE_CURVE ( ( 0.9999999999999991118, 0.8660254037844395958, 1.000000000000000000, 0.8660254037844387076, 1.000000000000000000, 0.9111405360107296403, 0.9401542295229903257 ) ) 
 REPRESENTATION_ITEM ( '' )  );
#7915 = EDGE_CURVE ( 'NONE', #7786, #998, #3114, .T. ) ;
#7916 = VERTEX_POINT ( 'NONE', #1202 ) ;
#7917 = PLANE ( 'NONE',  #9305 ) ;
#7918 = VERTEX_POINT ( 'NONE', #3312 ) ;
#7919 = DIRECTION ( 'NONE',  ( -1.000000000000000000, 0.000000000000000000, 0.000000000000000000 ) ) ;
#7920 = VECTOR ( 'NONE', #12384, 1000.000000000000000 ) ;
#7921 = VERTEX_POINT ( 'NONE', #2264 ) ;
#7922 = DIRECTION ( 'NONE',  ( -1.000000000000000000, 0.000000000000000000, -0.000000000000000000 ) ) ;
#7923 = EDGE_CURVE ( 'NONE', #5783, #5372, #12844, .T. ) ;
#7924 = ORIENTED_EDGE ( 'NONE', *, *, #12947, .T. ) ;
#7925 = EDGE_CURVE ( 'NONE', #7130, #8420, #12845, .T. ) ;
#7926 = DIRECTION ( 'NONE',  ( -0.000000000000000000, -0.000000000000000000, -1.000000000000000000 ) ) ;
#7927 = DIRECTION ( 'NONE',  ( -1.000000000000000000, 0.000000000000000000, 0.000000000000000000 ) ) ;
#7928 = LINE ( 'NONE', #3883, #9019 ) ;
#7929 = AXIS2_PLACEMENT_3D ( 'NONE', #10282, #7079, #256 ) ;
#7930 = CARTESIAN_POINT ( 'NONE',  ( 3.556430356250015024, 90.00000000000000000, 3.903125000614517504 ) ) ;
#7931 = VECTOR ( 'NONE', #465, 1000.000000000000000 ) ;
#7932 = DIRECTION ( 'NONE',  ( 0.000000000000000000, 0.000000000000000000, 1.000000000000000000 ) ) ;
#7933 = ORIENTED_EDGE ( 'NONE', *, *, #988, .F. ) ;
#7934 = CARTESIAN_POINT ( 'NONE',  ( 25.00000000000000355, -5.000000000000000000, 5.750000000000000000 ) ) ;
#7935 = ADVANCED_BREP_SHAPE_REPRESENTATION ( '', ( #3308, #5704 ), #466 ) ;
#7936 = CARTESIAN_POINT ( 'NONE',  ( 7.369500000000001272, 0.000000000000000000, 0.000000000000000000 ) ) ;
#7937 = CARTESIAN_POINT ( 'NONE',  ( 3.800000000000015365, 90.00000000000000000, 5.000000000000000000 ) ) ;
#7938 = VERTEX_POINT ( 'NONE', #5382 ) ;
#7939 = CIRCLE ( 'NONE', #6680, 32.70000000000000995 ) ;
#7940 = DIRECTION ( 'NONE',  ( 0.000000000000000000, 0.000000000000000000, 1.000000000000000000 ) ) ;
#7941 = ORIENTED_EDGE ( 'NONE', *, *, #10378, .F. ) ;
#7942 = PRODUCT_RELATED_PRODUCT_CATEGORY ( 'part', '', ( #282 ) ) ;
#7943 = CARTESIAN_POINT ( 'NONE',  ( 0.1038759689922479496, -3.348389132562988646, -0.8000000000000000444 ) ) ;
#7944 = CARTESIAN_POINT ( 'NONE',  ( 52.22659979626835991, 65.43896868087158225, -0.9999999999999970024 ) ) ;
#7945 = ORIENTED_EDGE ( 'NONE', *, *, #9262, .T. ) ;
#7946 = CARTESIAN_POINT ( 'NONE',  ( 19.27821517812503060, 62.76906990284727783, 3.584375000614516971 ) ) ;
#7947 = DIRECTION ( 'NONE',  ( 0.000000000000000000, 0.000000000000000000, -1.000000000000000000 ) ) ;
#7948 = PRODUCT_DEFINITION_SHAPE ( 'NONE', 'NONE',  #12972 ) ;
#7949 = EDGE_CURVE ( 'NONE', #11775, #4871, #4542, .T. ) ;
#7950 = VECTOR ( 'NONE', #9055, 1000.000000000000000 ) ;
#7951 = CARTESIAN_POINT ( 'NONE',  ( 25.00000000000000355, 2.000000000000000000, -5.750000000000000000 ) ) ;
#7952 = DIRECTION ( 'NONE',  ( -0.5000000000000043299, 0.8660254037844362651, 0.000000000000000000 ) ) ;
#7953 = FACE_OUTER_BOUND ( 'NONE', #174, .T. ) ;
#7954 = AXIS2_PLACEMENT_3D ( 'NONE', #4280, #8268, #11267 ) ;
#7955 = CYLINDRICAL_SURFACE ( 'NONE', #3364, 3.500000000000003109 ) ;
#7956 = CARTESIAN_POINT ( 'NONE',  ( 19.27821517812500574, 117.2309300971526937, 4.784375000614516260 ) ) ;
#7957 = ORIENTED_EDGE ( 'NONE', *, *, #1979, .T. ) ;
#7958 = EDGE_CURVE ( 'NONE', #362, #6201, #7548, .T. ) ;
#7959 = DIRECTION ( 'NONE',  ( -0.8660254037844361541, -0.5000000000000042188, 0.000000000000000000 ) ) ;
#7960 = ORIENTED_EDGE ( 'NONE', *, *, #6741, .T. ) ;
#7961 = ADVANCED_FACE ( 'NONE', ( #9576 ), #12386, .T. ) ;
#7962 = CARTESIAN_POINT ( 'NONE',  ( 50.00000000000000000, 0.000000000000000000, -10.00000000000000000 ) ) ;
#7963 = DIRECTION ( 'NONE',  ( 0.000000000000000000, 0.000000000000000000, -1.000000000000000000 ) ) ;
#7964 = CARTESIAN_POINT ( 'NONE',  ( 35.00000000000000000, 90.00000000000000000, 4.000000000000000000 ) ) ;
#7965 = CARTESIAN_POINT ( 'NONE',  ( 3.800000000000015365, 90.00000000000000000, 4.100000000000000533 ) ) ;
#7966 = EDGE_LOOP ( 'NONE', ( #3322, #8833, #7114, #6378 ) ) ;
#7967 = CYLINDRICAL_SURFACE ( 'NONE', #1994, 2.849999999999999201 ) ;
#7968 = DIRECTION ( 'NONE',  ( -0.000000000000000000, -0.000000000000000000, -1.000000000000000000 ) ) ;
#7969 = ORIENTED_EDGE ( 'NONE', *, *, #9052, .T. ) ;
#7970 = PRESENTATION_STYLE_ASSIGNMENT (( #3987 ) ) ;
#7971 = CARTESIAN_POINT ( 'NONE',  ( -48.33333333333332860, -5.000000000000000000, 1.499999999999999556 ) ) ;
#7972 = VERTEX_POINT ( 'NONE', #8470 ) ;
#7973 = EDGE_CURVE ( 'NONE', #9690, #4278, #10955, .T. ) ;
#7974 = AXIS2_PLACEMENT_3D ( 'NONE', #5691, #12434, #7588 ) ;
#7975 = CARTESIAN_POINT ( 'NONE',  ( -48.33333333333332860, 0.000000000000000000, 1.599999999999995426 ) ) ;
#7976 = ORIENTED_EDGE ( 'NONE', *, *, #1139, .F. ) ;
#7977 = CARTESIAN_POINT ( 'NONE',  ( 34.25000000000000000, 93.26496554346289258, -3.799999999999999822 ) ) ;
#7978 = FACE_OUTER_BOUND ( 'NONE', #9567, .T. ) ;
#7979 = EDGE_LOOP ( 'NONE', ( #8590, #1021 ) ) ;
#7980 = VERTEX_POINT ( 'NONE', #401 ) ;
#7981 =( GEOMETRIC_REPRESENTATION_CONTEXT ( 3 ) GLOBAL_UNCERTAINTY_ASSIGNED_CONTEXT ( ( #4240 ) ) GLOBAL_UNIT_ASSIGNED_CONTEXT ( ( #9677, #6729, #9618 ) ) REPRESENTATION_CONTEXT ( 'NONE', 'WORKASPACE' ) );
#7982 = DIRECTION ( 'NONE',  ( -0.000000000000000000, -0.000000000000000000, -1.000000000000000000 ) ) ;
#7983 = ORIENTED_EDGE ( 'NONE', *, *, #10637, .T. ) ;
#7984 = LINE ( 'NONE', #11968, #7094 ) ;
#7985 = VERTEX_POINT ( 'NONE', #10489 ) ;
#7986 = DIRECTION ( 'NONE',  ( -0.000000000000000000, 1.000000000000000000, -0.000000000000000000 ) ) ;
#7987 = ORIENTED_EDGE ( 'NONE', *, *, #12794, .F. ) ;
#7988 = EDGE_CURVE ( 'NONE', #8980, #8709, #7204, .T. ) ;
#7989 = DIRECTION ( 'NONE',  ( 1.000000000000000000, -0.000000000000000000, -0.000000000000000000 ) ) ;
#7990 = CARTESIAN_POINT ( 'NONE',  ( 3.556430356250028790, 71.84604660189818048, 3.940625000614517592 ) ) ;
#7991 =( NAMED_UNIT ( * ) PLANE_ANGLE_UNIT ( ) SI_UNIT ( $, .RADIAN. ) );
#7992 = AXIS2_PLACEMENT_3D ( 'NONE', #2575, #1783, #3562 ) ;
#7993 = CARTESIAN_POINT ( 'NONE',  ( 60.43447243729646345, 111.3420572890634048, 2.688859442485532991 ) ) ;
#7994 =( LENGTH_UNIT ( ) NAMED_UNIT ( * ) SI_UNIT ( .MILLI., .METRE. ) );
#7995 = CYLINDRICAL_SURFACE ( 'NONE', #8565, 3.500000000000003109 ) ;
#7996 = ADVANCED_FACE ( 'NONE', ( #3436 ), #8600, .F. ) ;
#7998 = ADVANCED_FACE ( 'NONE', ( #11405 ), #1596, .F. ) ;
#7997 = ORIENTED_EDGE ( 'NONE', *, *, #7347, .T. ) ;
#7999 = CARTESIAN_POINT ( 'NONE',  ( 64.29296370151269002, 100.7401778149417879, 3.000000000000000000 ) ) ;
#8000 = CYLINDRICAL_SURFACE ( 'NONE', #10854, 28.99999999999999289 ) ;
#8001 = CARTESIAN_POINT ( 'NONE',  ( 45.22164986280591847, 119.6006263581510183, 3.000000000000000444 ) ) ;
#8002 = ORIENTED_EDGE ( 'NONE', *, *, #1272, .T. ) ;
#8003 = AXIS2_PLACEMENT_3D ( 'NONE', #1767, #5756, #12505 ) ;
#8004 = DIRECTION ( 'NONE',  ( 0.000000000000000000, 0.000000000000000000, 1.000000000000000000 ) ) ;
#8005 = ORIENTED_EDGE ( 'NONE', *, *, #7250, .F. ) ;
#8006 = FACE_OUTER_BOUND ( 'NONE', #1713, .T. ) ;
#8007 = UNCERTAINTY_MEASURE_WITH_UNIT (LENGTH_MEASURE( 1.000000000000000082E-05 ), #7207, 'distance_accuracy_value', 'NONE');
#8008 = CARTESIAN_POINT ( 'NONE',  ( 50.72178482187499071, 117.2309300971526937, 4.203125000614517326 ) ) ;
#8009 = ORIENTED_EDGE ( 'NONE', *, *, #8568, .F. ) ;
#8010 = CARTESIAN_POINT ( 'NONE',  ( 50.72178482187499071, 117.2309300971526937, 3.359375000614517326 ) ) ;
#8011 = DIRECTION ( 'NONE',  ( 1.000000000000000000, 0.000000000000000000, -1.445602896647339656E-17 ) ) ;
#8012 = DIRECTION ( 'NONE',  ( -0.000000000000000000, -0.000000000000000000, -1.000000000000000000 ) ) ;
#8013 = DIRECTION ( 'NONE',  ( 0.000000000000000000, 0.000000000000000000, 1.000000000000000000 ) ) ;
#8014 = PRODUCT_DEFINITION ( 'UNKNOWN', '', #7609, #5679 ) ;
#8015 = VECTOR ( 'NONE', #8813, 1000.000000000000000 ) ;
#8016 = PLANE ( 'NONE',  #1974 ) ;
#8017 = CARTESIAN_POINT ( 'NONE',  ( -48.33333333333332860, -5.901290925839663970, -1.734723475976807094E-15 ) ) ;
#8018 = EDGE_CURVE ( 'NONE', #5609, #7529, #6778, .T. ) ;
#8019 = MECHANICAL_DESIGN_GEOMETRIC_PRESENTATION_REPRESENTATION (  '', ( #10095 ), #9472 ) ;
#8020 = CARTESIAN_POINT ( 'NONE',  ( 66.19999999999998863, 90.00000000000000000, 3.425000000000000266 ) ) ;
#8021 = CARTESIAN_POINT ( 'NONE',  ( 50.72178482187499071, 117.2309300971526937, 3.359375000614517326 ) ) ;
#8022 = VERTEX_POINT ( 'NONE', #9443 ) ;
#8023 = DIRECTION ( 'NONE',  ( -0.8660254037844360431, -0.5000000000000047740, -0.000000000000000000 ) ) ;
#8024 = EDGE_LOOP ( 'NONE', ( #9967, #8167, #8960, #5558 ) ) ;
#8025 = AXIS2_PLACEMENT_3D ( 'NONE', #2873, #4954, #953 ) ;
#8026 = LINE ( 'NONE', #11943, #4664 ) ;
#8027 = LINE ( 'NONE', #7008, #342 ) ;
#8028 = CARTESIAN_POINT ( 'NONE',  ( 20.00000000000000355, 121.2009999999999934, 1.500000000000000444 ) ) ;
#8030 = ADVANCED_FACE ( 'NONE', ( #467 ), #2650, .F. ) ;
#8029 = CARTESIAN_POINT ( 'NONE',  ( 5.000000000000004441, 30.00000000000000000, -2.500000000000000000 ) ) ;
#8031 = DIRECTION ( 'NONE',  ( 0.000000000000000000, 0.000000000000000000, 1.000000000000000000 ) ) ;
#8032 = EDGE_LOOP ( 'NONE', ( #6002, #10520, #7539 ) ) ;
#8033 = AXIS2_PLACEMENT_3D ( 'NONE', #9380, #12526, #10624 ) ;
#8034 = DIRECTION ( 'NONE',  ( -0.000000000000000000, 1.000000000000000000, -0.000000000000000000 ) ) ;
#8035 = EDGE_CURVE ( 'NONE', #11432, #10262, #8538, .T. ) ;
#8036 = CARTESIAN_POINT ( 'NONE',  ( 66.19999999999998863, 90.00000000000000000, 3.875000000000000000 ) ) ;
#8037 = AXIS2_PLACEMENT_3D ( 'NONE', #8735, #4939, #4029 ) ;
#8038 = ORIENTED_EDGE ( 'NONE', *, *, #9088, .F. ) ;
#8039 = DIRECTION ( 'NONE',  ( -0.000000000000000000, 1.000000000000000000, -0.000000000000000000 ) ) ;
#8040 = ORIENTED_EDGE ( 'NONE', *, *, #4700, .F. ) ;
#8041 = SURFACE_STYLE_USAGE ( .BOTH. , #4839 ) ;
#8042 = ORIENTED_EDGE ( 'NONE', *, *, #12633, .T. ) ;
#8043 = DIRECTION ( 'NONE',  ( -1.000000000000000000, 0.000000000000000000, 0.000000000000000000 ) ) ;
#8044 = CARTESIAN_POINT ( 'NONE',  ( 21.49999999999998579, 90.00000000000000000, -10.00000000000000178 ) ) ;
#8045 = VECTOR ( 'NONE', #700, 1000.000000000000000 ) ;
#8046 = ORIENTED_EDGE ( 'NONE', *, *, #3656, .F. ) ;
#8047 = AXIS2_PLACEMENT_3D ( 'NONE', #9829, #4925, #10810 ) ;
#8048 = EDGE_CURVE ( 'NONE', #39, #1413, #1131, .T. ) ;
#8049 = ORIENTED_EDGE ( 'NONE', *, *, #9345, .F. ) ;
#8050 = DIRECTION ( 'NONE',  ( -1.000000000000000000, 0.000000000000000000, 0.000000000000000000 ) ) ;
#8051 = ORIENTED_EDGE ( 'NONE', *, *, #1839, .T. ) ;
#8052 = CARTESIAN_POINT ( 'NONE',  ( 35.00000000000000000, 126.3079067962035822, 3.340625000614517059 ) ) ;
#8053 = ORIENTED_EDGE ( 'NONE', *, *, #2569, .F. ) ;
#8054 = AXIS2_PLACEMENT_3D ( 'NONE', #5019, #889, #3065 ) ;
#8055 = CARTESIAN_POINT ( 'NONE',  ( 35.00000000000000711, 53.97334320256736362, 3.425000001229034474 ) ) ;
#8056 = VERTEX_POINT ( 'NONE', #10622 ) ;
#8057 = VECTOR ( 'NONE', #7785, 1000.000000000000000 ) ;
#8058 = DIRECTION ( 'NONE',  ( 0.000000000000000000, 0.000000000000000000, -1.000000000000000000 ) ) ;
#8059 = CARTESIAN_POINT ( 'NONE',  ( 66.44356964375000985, 71.84604660189820891, 4.540625000614517681 ) ) ;
#8060 = CARTESIAN_POINT ( 'NONE',  ( 3.800000000000015365, 90.00000000000000000, 5.000000000000000000 ) ) ;
#8061 = CARTESIAN_POINT ( 'NONE',  ( 60.00000000000000000, -6.000000000000000000, 15.00000000000000000 ) ) ;
#8062 = CARTESIAN_POINT ( 'NONE',  ( 45.00000000000000000, 3.649999999999993694, 5.750000000000000888 ) ) ;
#8063 = FACE_BOUND ( 'NONE', #4231, .T. ) ;
#8064 = EDGE_CURVE ( 'NONE', #9137, #3599, #1525, .T. ) ;
#8065 = ORIENTED_EDGE ( 'NONE', *, *, #666, .T. ) ;
#8066 = CARTESIAN_POINT ( 'NONE',  ( 35.00000000000000000, 126.3079067962035822, 4.746875000614517504 ) ) ;
#8067 = DIRECTION ( 'NONE',  ( -0.000000000000000000, 0.000000000000000000, 1.000000000000000000 ) ) ;
#8068 = CARTESIAN_POINT ( 'NONE',  ( 63.34962933878586711, 103.3078946294862135, 3.000000000000001776 ) ) ;
#8069 = ORIENTED_EDGE ( 'NONE', *, *, #3723, .F. ) ;
#8070 = FACE_OUTER_BOUND ( 'NONE', #12240, .T. ) ;
#8071 = VERTEX_POINT ( 'NONE', #4672 ) ;
#8072 = DIRECTION ( 'NONE',  ( -1.000000000000000000, -0.000000000000000000, -0.000000000000000000 ) ) ;
#8073 = CARTESIAN_POINT ( 'NONE',  ( 66.44356964374998142, 108.1539533981018053, 3.265625000614516882 ) ) ;
#8075 = EDGE_CURVE ( 'NONE', #5822, #4697, #3568, .T. ) ;
#8074 = VERTEX_POINT ( 'NONE', #12523 ) ;
#8076 = EDGE_CURVE ( 'NONE', #454, #1278, #2823, .T. ) ;
#8077 = CARTESIAN_POINT ( 'NONE',  ( 60.43447242791587826, 111.3420572944792895, 3.026359441279048657 ) ) ;
#8078 = LINE ( 'NONE', #11136, #11860 ) ;
#8079 = FACE_BOUND ( 'NONE', #7979, .T. ) ;
#8080 = PLANE ( 'NONE',  #2411 ) ;
#8081 = EDGE_CURVE ( 'NONE', #2507, #865, #3460, .T. ) ;
#8082 = DIRECTION ( 'NONE',  ( -0.000000000000000000, -0.000000000000000000, -1.000000000000000000 ) ) ;
#8083 = AXIS2_PLACEMENT_3D ( 'NONE', #1388, #5375, #9371 ) ;
#8084 = CARTESIAN_POINT ( 'NONE',  ( 4.270088556250601699E-16, 30.00000000000000000, -8.000000000000000000 ) ) ;
#8085 = DIRECTION ( 'NONE',  ( -0.000000000000000000, -0.000000000000000000, -1.000000000000000000 ) ) ;
#8086 = DIRECTION ( 'NONE',  ( -0.000000000000000000, 1.000000000000000000, -0.000000000000000000 ) ) ;
#8087 = VERTEX_POINT ( 'NONE', #5896 ) ;
#8088 = EDGE_CURVE ( 'NONE', #5076, #9939, #1561, .T. ) ;
#8089 = CARTESIAN_POINT ( 'NONE',  ( 1.649999999999999023, 1.499999999999997113, 0.000000000000000000 ) ) ;
#8090 = ORIENTED_EDGE ( 'NONE', *, *, #6990, .F. ) ;
#8091 = DIRECTION ( 'NONE',  ( -0.000000000000000000, 1.000000000000000000, -0.000000000000000000 ) ) ;
#8092 = DIRECTION ( 'NONE',  ( 0.5877852522924715828, 0.8090169943749485615, 0.000000000000000000 ) ) ;
#8093 = DIRECTION ( 'NONE',  ( 0.8660254037844361541, 0.5000000000000042188, 9.389466242107209433E-17 ) ) ;
#8094 = ORIENTED_EDGE ( 'NONE', *, *, #440, .T. ) ;
#8095 = ADVANCED_BREP_SHAPE_REPRESENTATION ( '', ( #11745, #5704 ), #898 ) ;
#8096 = CARTESIAN_POINT ( 'NONE',  ( 35.00000000000000000, 90.00000000000000000, 4.000000000000000000 ) ) ;
#8097 = CARTESIAN_POINT ( 'NONE',  ( 8.500000000000000000, 69.54849343948981755, -1.000000000000000666 ) ) ;
#8098 = CIRCLE ( 'NONE', #10813, 0.7499999999999997780 ) ;
#8099 = VERTEX_POINT ( 'NONE', #8909 ) ;
#8100 =( NAMED_UNIT ( * ) PLANE_ANGLE_UNIT ( ) SI_UNIT ( $, .RADIAN. ) );
#8101 = SURFACE_STYLE_FILL_AREA ( #4113 ) ;
#8102 = VERTEX_POINT ( 'NONE', #3444 ) ;
#8103 = APPLICATION_CONTEXT ( 'automotive_design' ) ;
#8104 = FACE_OUTER_BOUND ( 'NONE', #5426, .T. ) ;
#8105 = ORIENTED_EDGE ( 'NONE', *, *, #12071, .T. ) ;
#8106 = CARTESIAN_POINT ( 'NONE',  ( -0.9999999999999997780, -4.273461295629625845, 0.000000000000000000 ) ) ;
#8107 =( BOUNDED_SURFACE ( )  B_SPLINE_SURFACE ( 1, 2, ( 
 ( #9707, #11736, #12597, #2785, #804, #1798, #3900, #3706, #10754, #5784, #11806, #11613, #10570, #3768, #1606, #1670, #612, #12787, #5592, #744, #3641, #4869, #9775, #4744, #5720, #8730, #2659, #4808, #6633, #3831, #9585, #6764, #2853, #4618, #6825, #10819, #1864, #12726, #8858, #9838, #5656, #4680, #11543, #7748, #868, #12852, #8668, #2590, #11675, #2723, #6697, #10692, #1733, #8077, #6168 ),
 ( #5189, #9178, #8922, #7025, #3042, #11867, #6957, #2914, #11135, #11993, #2976, #7091, #3109, #9046, #10881, #4, #11072, #5907, #4026, #73, #2191, #201, #6894, #6038, #12062, #4937, #2124, #10091, #6100, #7880, #8981, #1127, #5121, #4152, #7946, #9113, #10161, #12916, #5055, #11006, #8010, #137, #1993, #3962, #8143, #11932, #5973, #12129, #10943, #9968, #4088, #3175, #1926, #999, #7152 ) ),
 .UNSPECIFIED., .F., .F., .F. ) 
 B_SPLINE_SURFACE_WITH_KNOTS ( ( 2, 2 ),
 ( 3, 2, 2, 2, 2, 2, 2, 2, 2, 2, 2, 2, 2, 2, 2, 2, 2, 2, 2, 2, 2, 2, 2, 2, 2, 2, 2, 3 ),
 ( 0.000000000000000000, 1.000000000000000000 ),
 ( 0.000000000000000000, 0.03333333333333333287, 0.06666666666666666574, 0.1000000000000000056, 0.1333333333333333315, 0.1666666666666666574, 0.2000000000000000111, 0.2333333333333333370, 0.2666666666666666630, 0.2999999999999999889, 0.3333333333333333148, 0.3666666666666666408, 0.4000000000000000222, 0.4333333333333333481, 0.4666666666666666741, 0.5000000000000000000, 0.5333333333333333259, 0.5666666666666666519, 0.5999999999999999778, 0.6333333333333333037, 0.6666666666666666297, 0.6999999999999999556, 0.7333333333333332815, 0.7666666666666667185, 0.8000000000000000444, 0.8333333333333333703, 0.8666666666666666963, 0.8887752010443024098 ),
 .UNSPECIFIED. ) 
 GEOMETRIC_REPRESENTATION_ITEM ( )  RATIONAL_B_SPLINE_SURFACE ( (
 ( 1.000000000000000000, 0.8660254037844387076, 1.000000000000000000, 0.8660254037844387076, 1.000000000000000000, 0.8660254037844387076, 1.000000000000000000, 0.8660254037844387076, 1.000000000000000000, 0.8660254037844387076, 1.000000000000000000, 0.8660254037844387076, 1.000000000000000000, 0.8660254037844387076, 1.000000000000000000, 0.8660254037844387076, 1.000000000000000000, 0.8660254037844387076, 1.000000000000000000, 0.8660254037844387076, 1.000000000000000000, 0.8660254037844387076, 1.000000000000000000, 0.8660254037844387076, 1.000000000000000000, 0.8660254037844387076, 1.000000000000000000, 0.8660254037844387076, 1.000000000000000000, 0.8660254037844387076, 1.000000000000000000, 0.8660254037844387076, 1.000000000000000000, 0.8660254037844387076, 1.000000000000000000, 0.8660254037844387076, 1.000000000000000000, 0.8660254037844387076, 1.000000000000000000, 0.8660254037844387076, 1.000000000000000000, 0.8660254037844387076, 1.000000000000000000, 0.8660254037844387076, 1.000000000000000000, 0.8660254037844387076, 1.000000000000000000, 0.8660254037844387076, 1.000000000000000000, 0.8660254037844387076, 1.000000000000000000, 0.8660254037844387076, 1.000000000000000000, 0.9111405410151519613, 0.9401542262549813511),
 ( 1.000000000000000000, 0.8660254037844387076, 1.000000000000000000, 0.8660254037844387076, 1.000000000000000000, 0.8660254037844387076, 1.000000000000000000, 0.8660254037844387076, 1.000000000000000000, 0.8660254037844387076, 1.000000000000000000, 0.8660254037844387076, 1.000000000000000000, 0.8660254037844387076, 1.000000000000000000, 0.8660254037844387076, 1.000000000000000000, 0.8660254037844387076, 1.000000000000000000, 0.8660254037844387076, 1.000000000000000000, 0.8660254037844387076, 1.000000000000000000, 0.8660254037844387076, 1.000000000000000000, 0.8660254037844387076, 1.000000000000000000, 0.8660254037844387076, 1.000000000000000000, 0.8660254037844387076, 1.000000000000000000, 0.8660254037844387076, 1.000000000000000000, 0.8660254037844387076, 1.000000000000000000, 0.8660254037844387076, 1.000000000000000000, 0.8660254037844387076, 1.000000000000000000, 0.8660254037844387076, 1.000000000000000000, 0.8660254037844387076, 1.000000000000000000, 0.8660254037844387076, 1.000000000000000000, 0.8660254037844387076, 1.000000000000000000, 0.8660254037844387076, 1.000000000000000000, 0.8660254037844387076, 1.000000000000000000, 0.8660254037844387076, 1.000000000000000000, 0.9111405410151519613, 0.9401542262549813511) ) ) 
 REPRESENTATION_ITEM ( '' )  SURFACE ( )  );
#8108 = FACE_OUTER_BOUND ( 'NONE', #11882, .T. ) ;
#8109 = EDGE_CURVE ( 'NONE', #7130, #4396, #4016, .T. ) ;
#8110 = ORIENTED_EDGE ( 'NONE', *, *, #12070, .F. ) ;
#8111 = CIRCLE ( 'NONE', #6850, 1.000000000000000000 ) ;
#8112 = EDGE_LOOP ( 'NONE', ( #10957, #12031, #6970, #4465 ) ) ;
#8113 = FACE_OUTER_BOUND ( 'NONE', #5079, .T. ) ;
#8114 = VERTEX_POINT ( 'NONE', #1790 ) ;
#8115 = DIRECTION ( 'NONE',  ( -1.000000000000000000, 0.000000000000000000, 0.000000000000000000 ) ) ;
#8116 = CARTESIAN_POINT ( 'NONE',  ( 64.54728994471078352, 100.7543353520590870, 2.802601390178781404 ) ) ;
#8117 = VERTEX_POINT ( 'NONE', #11727 ) ;
#8118 = FACE_BOUND ( 'NONE', #518, .T. ) ;
#8119 = DIRECTION ( 'NONE',  ( 0.5000000000000049960, -0.8660254037844357100, 0.000000000000000000 ) ) ;
#8120 = EDGE_LOOP ( 'NONE', ( #6525, #3655 ) ) ;
#8121 = AXIS2_PLACEMENT_3D ( 'NONE', #4441, #8370, #9343 ) ;
#8122 = DIRECTION ( 'NONE',  ( -1.000000000000000000, -0.000000000000000000, -0.000000000000000000 ) ) ;
#8123 = FACE_OUTER_BOUND ( 'NONE', #10281, .T. ) ;
#8124 = EDGE_CURVE ( 'NONE', #7014, #8561, #4491, .T. ) ;
#8125 = CARTESIAN_POINT ( 'NONE',  ( 66.19999999999993179, 71.98667160128364628, 3.500000001229034208 ) ) ;
#8126 = CARTESIAN_POINT ( 'NONE',  ( 50.60000000000001563, 62.98000740192552627, 3.012500001229034829 ) ) ;
#8127 = EDGE_CURVE ( 'NONE', #1488, #11890, #4735, .T. ) ;
#8128 = PLANE ( 'NONE',  #11046 ) ;
#8129 = AXIS2_PLACEMENT_3D ( 'NONE', #180, #3219, #4132 ) ;
#8130 = VERTEX_POINT ( 'NONE', #3821 ) ;
#8131 = CARTESIAN_POINT ( 'NONE',  ( 35.00000000000000000, 126.0266567974326222, 4.437500000000000888 ) ) ;
#8132 = CARTESIAN_POINT ( 'NONE',  ( 25.00000000000000355, 0.000000000000000000, 7.349999999999996980 ) ) ;
#8133 = CYLINDRICAL_SURFACE ( 'NONE', #1776, 0.7499999999999997780 ) ;
#8134 = ORIENTED_EDGE ( 'NONE', *, *, #11408, .F. ) ;
#8135 = LINE ( 'NONE', #4338, #11562 ) ;
#8136 = VERTEX_POINT ( 'NONE', #11982 ) ;
#8137 = CIRCLE ( 'NONE', #6662, 29.99999999999999645 ) ;
#8138 = CARTESIAN_POINT ( 'NONE',  ( 21.49999999999998579, 90.00000000000000000, -10.00000000000000000 ) ) ;
#8139 = CARTESIAN_POINT ( 'NONE',  ( 38.50000000000000711, 90.00000000000000000, 6.000000000000000000 ) ) ;
#8140 = ORIENTED_EDGE ( 'NONE', *, *, #2025, .T. ) ;
#8141 = EDGE_CURVE ( 'NONE', #4442, #3844, #6760, .T. ) ;
#8142 = VECTOR ( 'NONE', #10488, 1000.000000000000000 ) ;
#8143 = CARTESIAN_POINT ( 'NONE',  ( 50.72178482187501203, 62.76906990284730625, 3.209375000614517415 ) ) ;
#8144 = CARTESIAN_POINT ( 'NONE',  ( 35.75000000000000711, 93.41869858279433458, 6.000000000000000000 ) ) ;
#8145 = DIRECTION ( 'NONE',  ( -1.000000000000000000, 0.000000000000000000, 0.000000000000000000 ) ) ;
#8146 = AXIS2_PLACEMENT_3D ( 'NONE', #3361, #9036, #63 ) ;
#8147 = CARTESIAN_POINT ( 'NONE',  ( 35.00000000000000000, 90.00000000000000000, -8.000000000000000000 ) ) ;
#8148 = CARTESIAN_POINT ( 'NONE',  ( 35.49999999999999289, 96.48074069840785683, 22.38477631085024555 ) ) ;
#8149 = DIRECTION ( 'NONE',  ( 1.914177628664063178E-15, -1.000000000000000000, 0.000000000000000000 ) ) ;
#8150 = DIRECTION ( 'NONE',  ( -0.000000000000000000, -0.000000000000000000, -1.000000000000000000 ) ) ;
#8151 = LINE ( 'NONE', #12863, #11284 ) ;
#8152 = CARTESIAN_POINT ( 'NONE',  ( 66.44356964374998142, 108.1539533981018053, 3.321875000614517237 ) ) ;
#8153 = VERTEX_POINT ( 'NONE', #10931 ) ;
#8154 = VECTOR ( 'NONE', #12497, 1000.000000000000000 ) ;
#8155 = CARTESIAN_POINT ( 'NONE',  ( -16.33333333333332504, 2.000000000000000000, 7.999999999999996447 ) ) ;
#8156 = ORIENTED_EDGE ( 'NONE', *, *, #9390, .T. ) ;
#8157 = ADVANCED_FACE ( 'NONE', ( #7740 ), #1723, .F. ) ;
#8158 = CARTESIAN_POINT ( 'NONE',  ( -63.73205080756886076, 30.46410161513775350, 0.000000000000000000 ) ) ;
#8159 = DIRECTION ( 'NONE',  ( -0.000000000000000000, 1.000000000000000000, -0.000000000000000000 ) ) ;
#8160 = EDGE_CURVE ( 'NONE', #11257, #8414, #11799, .T. ) ;
#8161 = CARTESIAN_POINT ( 'NONE',  ( 25.00000000000000355, 0.000000000000000000, 5.750000000000000000 ) ) ;
#8162 = ADVANCED_FACE ( 'NONE', ( #12779, #12905, #11794 ), #6883, .T. ) ;
#8163 = AXIS2_PLACEMENT_3D ( 'NONE', #5981, #5199, #2068 ) ;
#8164 = ORIENTED_EDGE ( 'NONE', *, *, #3372, .F. ) ;
#8165 = LINE ( 'NONE', #8421, #3469 ) ;
#8166 = CARTESIAN_POINT ( 'NONE',  ( 35.00000000000000000, 90.00000000000000000, 3.000000000000000000 ) ) ;
#8167 = ORIENTED_EDGE ( 'NONE', *, *, #1929, .T. ) ;
#8168 = CARTESIAN_POINT ( 'NONE',  ( 9.650000000000000355, 0.000000000000000000, 0.000000000000000000 ) ) ;
#8169 = ORIENTED_EDGE ( 'NONE', *, *, #994, .F. ) ;
#8170 = ORIENTED_EDGE ( 'NONE', *, *, #2943, .F. ) ;
#8171 = CARTESIAN_POINT ( 'NONE',  ( 60.00000000000000000, -6.000000000000000000, 15.00000000000000000 ) ) ;
#8172 = VECTOR ( 'NONE', #10627, 1000.000000000000114 ) ;
#8173 = DIRECTION ( 'NONE',  ( -0.000000000000000000, -0.000000000000000000, -1.000000000000000000 ) ) ;
#8174 = ORIENTED_EDGE ( 'NONE', *, *, #4232, .F. ) ;
#8175 = ORIENTED_EDGE ( 'NONE', *, *, #12241, .F. ) ;
#8176 = FACE_OUTER_BOUND ( 'NONE', #8670, .T. ) ;
#8177 = VERTEX_POINT ( 'NONE', #5840 ) ;
#8178 = CARTESIAN_POINT ( 'NONE',  ( 35.00000000000000711, 53.69209320379640360, 4.465625000614517504 ) ) ;
#8179 = VERTEX_POINT ( 'NONE', #10684 ) ;
#8180 = VECTOR ( 'NONE', #8058, 1000.000000000000000 ) ;
#8181 = DIRECTION ( 'NONE',  ( -0.000000000000000000, -0.000000000000000000, -1.000000000000000000 ) ) ;
#8182 = EDGE_CURVE ( 'NONE', #7595, #6209, #9957, .T. ) ;
#8183 = DIRECTION ( 'NONE',  ( -1.000000000000000000, 0.000000000000000000, 0.000000000000000000 ) ) ;
#8184 = ORIENTED_EDGE ( 'NONE', *, *, #11359, .F. ) ;
#8185 =( BOUNDED_CURVE ( )  B_SPLINE_CURVE ( 2, ( #2999, #5078, #12151, #10967, #9071, #1152, #7246 ),
 .UNSPECIFIED., .F., .F. ) 
 B_SPLINE_CURVE_WITH_KNOTS ( ( 3, 2, 2, 3 ),
 ( 0.1999999999999999833, 0.2333333333333333925, 0.2666666666666668295, 0.3000000000000002109 ),
 .UNSPECIFIED. ) 
 CURVE ( )  GEOMETRIC_REPRESENTATION_ITEM ( )  RATIONAL_B_SPLINE_CURVE ( ( 1.000000000000000222, 0.8660254037844385966, 1.000000000000000000, 0.8660254037844387076, 1.000000000000000000, 0.8660254037844378194, 1.000000000000000888 ) ) 
 REPRESENTATION_ITEM ( '' )  );
#8186 = CARTESIAN_POINT ( 'NONE',  ( 1.040000000000000036, -0.5773502691896253980, 1.000000000000000000 ) ) ;
#8187 = CARTESIAN_POINT ( 'NONE',  ( 19.27821517812503060, 62.76906990284727783, 4.428125000614516971 ) ) ;
#8188 = LINE ( 'NONE', #12175, #5479 ) ;
#8189 = CARTESIAN_POINT ( 'NONE',  ( 66.20000000000000284, 71.98667160128370313, 3.050000001229034474 ) ) ;
#8190 = MECHANICAL_DESIGN_GEOMETRIC_PRESENTATION_REPRESENTATION (  '', ( #6706 ), #7981 ) ;
#8191 = FACE_BOUND ( 'NONE', #11129, .T. ) ;
#8192 = EDGE_LOOP ( 'NONE', ( #6289, #9552, #4663, #2881 ) ) ;
#8193 = CARTESIAN_POINT ( 'NONE',  ( 35.00000000000000000, 126.0266567974326222, 3.537500000000000089 ) ) ;
#8194 = EDGE_CURVE ( 'NONE', #8368, #1906, #11164, .T. ) ;
#8195 = ORIENTED_EDGE ( 'NONE', *, *, #4002, .T. ) ;
#8196 = DIRECTION ( 'NONE',  ( 1.000000000000000000, 0.000000000000000000, 2.891205793294678696E-17 ) ) ;
#8197 = ORIENTED_EDGE ( 'NONE', *, *, #11930, .T. ) ;
#8198 = CARTESIAN_POINT ( 'NONE',  ( 35.00000000000000000, 90.00000000000000000, 5.000000000000000000 ) ) ;
#8199 = ADVANCED_FACE ( 'NONE', ( #5711 ), #4082, .F. ) ;
#8200 = EDGE_LOOP ( 'NONE', ( #907, #8156 ) ) ;
#8201 = CIRCLE ( 'NONE', #8621, 4.000000000000003553 ) ;
#8202 = CARTESIAN_POINT ( 'NONE',  ( 35.00000000000000000, 90.00000000000000000, 4.000000000000000000 ) ) ;
#8203 = CARTESIAN_POINT ( 'NONE',  ( 66.44356964374999563, 71.84604660189820891, 3.640625000614517326 ) ) ;
#8204 = ORIENTED_EDGE ( 'NONE', *, *, #10513, .F. ) ;
#8205 = CARTESIAN_POINT ( 'NONE',  ( 3.556430356250015024, 90.00000000000000000, 3.059375000614517059 ) ) ;
#8206 = DIRECTION ( 'NONE',  ( -0.8660254037844362651, -0.5000000000000042188, 0.000000000000000000 ) ) ;
#8207 = CYLINDRICAL_SURFACE ( 'NONE', #6653, 3.500000000000003109 ) ;
#8208 = VECTOR ( 'NONE', #5543, 1000.000000000000000 ) ;
#8209 = PRESENTATION_STYLE_ASSIGNMENT (( #11277 ) ) ;
#8210 = EDGE_CURVE ( 'NONE', #7875, #5463, #8846, .T. ) ;
#8211 = LINE ( 'NONE', #2265, #4402 ) ;
#8212 = FACE_BOUND ( 'NONE', #5224, .T. ) ;
#8213 = LINE ( 'NONE', #12201, #4722 ) ;
#8214 = CARTESIAN_POINT ( 'NONE',  ( 35.00000000000000000, 90.00000000000000000, 6.000000000000000000 ) ) ;
#8215 = CARTESIAN_POINT ( 'NONE',  ( 66.44356964374998142, 108.1539533981018053, 3.771875000614516082 ) ) ;
#8216 = ORIENTED_EDGE ( 'NONE', *, *, #11202, .F. ) ;
#8217 = DIRECTION ( 'NONE',  ( -0.000000000000000000, 0.000000000000000000, -1.000000000000000000 ) ) ;
#8218 = ORIENTED_EDGE ( 'NONE', *, *, #1382, .F. ) ;
#8219 =( LENGTH_UNIT ( ) NAMED_UNIT ( * ) SI_UNIT ( .MILLI., .METRE. ) );
#8220 = CARTESIAN_POINT ( 'NONE',  ( -57.99999999999999289, 30.00000000000000000, 7.999999999999996447 ) ) ;
#8221 = CYLINDRICAL_SURFACE ( 'NONE', #1149, 1.500000000000001332 ) ;
#8222 = ADVANCED_FACE ( 'NONE', ( #2905 ), #10593, .F. ) ;
#8223 = CARTESIAN_POINT ( 'NONE',  ( 36.58116973490655255, 87.04662866042625069, -3.799999999999999822 ) ) ;
#8224 = MECHANICAL_DESIGN_GEOMETRIC_PRESENTATION_REPRESENTATION (  '', ( #11566 ), #7391 ) ;
#8225 = EDGE_LOOP ( 'NONE', ( #6064, #5505, #5247, #6414 ) ) ;
#8226 = DIRECTION ( 'NONE',  ( 0.000000000000000000, 0.000000000000000000, 1.000000000000000000 ) ) ;
#8227 = CARTESIAN_POINT ( 'NONE',  ( 8.499999999999998224, 71.85789451624832225, 1.000000000000000444 ) ) ;
#8228 = ORIENTED_EDGE ( 'NONE', *, *, #9782, .T. ) ;
#8229 = AXIS2_PLACEMENT_3D ( 'NONE', #3063, #7834, #12747 ) ;
#8230 = LINE ( 'NONE', #297, #6391 ) ;
#8231 = ORIENTED_EDGE ( 'NONE', *, *, #9402, .F. ) ;
#8232 = ORIENTED_EDGE ( 'NONE', *, *, #8450, .F. ) ;
#8233 = ADVANCED_FACE ( 'NONE', ( #12374 ), #450, .F. ) ;
#8234 = EDGE_CURVE ( 'NONE', #2240, #11750, #8519, .T. ) ;
#8235 = CARTESIAN_POINT ( 'NONE',  ( 19.40000000000000924, 117.0199925980744666, 2.787500001229034297 ) ) ;
#8236 = CARTESIAN_POINT ( 'NONE',  ( 52.49999999999996447, 94.00000000000000000, -8.000000000000000000 ) ) ;
#8237 = DIRECTION ( 'NONE',  ( -0.8660254037844361541, -0.5000000000000042188, 0.000000000000000000 ) ) ;
#8238 = ORIENTED_EDGE ( 'NONE', *, *, #5067, .F. ) ;
#8239 = VECTOR ( 'NONE', #4814, 1000.000000000000000 ) ;
#8240 = ORIENTED_EDGE ( 'NONE', *, *, #11663, .F. ) ;
#8241 = CIRCLE ( 'NONE', #1341, 4.338286831716297698 ) ;
#8242 = FACE_BOUND ( 'NONE', #1287, .T. ) ;
#8243 = ORIENTED_EDGE ( 'NONE', *, *, #6771, .T. ) ;
#8244 = EDGE_CURVE ( 'NONE', #9021, #11182, #4287, .T. ) ;
#8245 = PRODUCT_CONTEXT ( 'NONE', #6170, 'mechanical' ) ;
#8246 = CARTESIAN_POINT ( 'NONE',  ( 66.44356964374998142, 108.1539533981018053, 3.265625000614516882 ) ) ;
#8247 = EDGE_LOOP ( 'NONE', ( #5767, #784, #2007, #5606 ) ) ;
#8248 = DIRECTION ( 'NONE',  ( 1.000000000000000000, 0.000000000000000000, 0.000000000000000000 ) ) ;
#8249 = LINE ( 'NONE', #11114, #11256 ) ;
#8250 = ORIENTED_EDGE ( 'NONE', *, *, #9626, .T. ) ;
#8251 = CARTESIAN_POINT ( 'NONE',  ( 1.649999999999999911, 0.000000000000000000, 0.000000000000000000 ) ) ;
#8252 = AXIS2_PLACEMENT_3D ( 'NONE', #8438, #7144, #3100 ) ;
#8253 = AXIS2_PLACEMENT_3D ( 'NONE', #4474, #5583, #3698 ) ;
#8254 = CARTESIAN_POINT ( 'NONE',  ( 45.00000000000000000, -5.000000000000000000, -7.250000000000000888 ) ) ;
#8255 = CARTESIAN_POINT ( 'NONE',  ( 66.19999999999998863, 90.00000000000000000, 3.537500001229034297 ) ) ;
#8256 = PRESENTATION_STYLE_ASSIGNMENT (( #5430 ) ) ;
#8257 = DIRECTION ( 'NONE',  ( -1.000000000000000000, 0.000000000000000000, 0.000000000000000000 ) ) ;
#8258 = EDGE_CURVE ( 'NONE', #10818, #12910, #11925, .T. ) ;
#8259 = ORIENTED_EDGE ( 'NONE', *, *, #7690, .T. ) ;
#8260 = CARTESIAN_POINT ( 'NONE',  ( 66.20000000000000284, 71.98667160128370313, 4.737500000000000711 ) ) ;
#8261 = ORIENTED_EDGE ( 'NONE', *, *, #8949, .T. ) ;
#8262 = CIRCLE ( 'NONE', #12653, 1.499999999999999556 ) ;
#8263 = CARTESIAN_POINT ( 'NONE',  ( 3.800000000000135270, 108.0133283987163679, 3.162500000000000533 ) ) ;
#8264 = ORIENTED_EDGE ( 'NONE', *, *, #5821, .F. ) ;
#8265 = AXIS2_PLACEMENT_3D ( 'NONE', #4969, #12232, #2097 ) ;
#8266 = FACE_OUTER_BOUND ( 'NONE', #4247, .T. ) ;
#8267 = VERTEX_POINT ( 'NONE', #10412 ) ;
#8268 = DIRECTION ( 'NONE',  ( -1.000000000000000000, -0.000000000000000000, -0.000000000000000000 ) ) ;
#8269 = CARTESIAN_POINT ( 'NONE',  ( 50.72178482187499071, 117.2309300971526937, 2.853125000614517237 ) ) ;
#8270 = CARTESIAN_POINT ( 'NONE',  ( 66.44356964374999563, 90.00000000000000000, 4.634375000614516793 ) ) ;
#8271 = DIRECTION ( 'NONE',  ( -0.000000000000000000, 1.000000000000000000, -0.000000000000000000 ) ) ;
#8272 = VECTOR ( 'NONE', #2922, 1000.000000000000000 ) ;
#8273 = DIRECTION ( 'NONE',  ( 0.000000000000000000, 0.000000000000000000, 1.000000000000000000 ) ) ;
#8274 = VECTOR ( 'NONE', #9527, 1000.000000000000000 ) ;
#8275 = EDGE_CURVE ( 'NONE', #12575, #5463, #1447, .T. ) ;
#8276 = LINE ( 'NONE', #10233, #3337 ) ;
#8277 = DIRECTION ( 'NONE',  ( -0.000000000000000000, -0.000000000000000000, -1.000000000000000000 ) ) ;
#8278 = CIRCLE ( 'NONE', #2646, 2.849999999999999645 ) ;
#8279 = DIRECTION ( 'NONE',  ( -0.5000000000000043299, 0.8660254037844362651, 0.000000000000000000 ) ) ;
#8280 = PRESENTATION_LAYER_ASSIGNMENT (  '', '', ( #10789 ) ) ;
#8281 = CARTESIAN_POINT ( 'NONE',  ( 1.750000000000000000, 1.959434878635764737E-16, -1.599999999999999645 ) ) ;
#8282 = CARTESIAN_POINT ( 'NONE',  ( 8.999999999999989342, 72.14656965084313356, 1.000000000000000000 ) ) ;
#8283 = EDGE_LOOP ( 'NONE', ( #7709, #10392, #6647, #12364, #4786, #11169, #6399 ) ) ;
#8284 = DIRECTION ( 'NONE',  ( 5.337610695313252124E-17, 0.000000000000000000, -1.000000000000000000 ) ) ;
#8285 = ORIENTED_EDGE ( 'NONE', *, *, #6671, .T. ) ;
#8286 = EDGE_CURVE ( 'NONE', #5406, #9676, #3488, .T. ) ;
#8287 = SHAPE_REPRESENTATION_RELATIONSHIP ( 'NONE' , 'NONE' ,  #985, #2170 ) ;
#8288 = ADVANCED_FACE ( 'NONE', ( #1772 ), #10797, .F. ) ;
#8289 = VECTOR ( 'NONE', #9056, 1000.000000000000114 ) ;
#8290 = CARTESIAN_POINT ( 'NONE',  ( 46.98957880828161393, 117.5000000000000711, -0.9999999999999970024 ) ) ;
#8291 = CARTESIAN_POINT ( 'NONE',  ( 4.999999999999962697, 79.07477288111861924, 3.000000000000000000 ) ) ;
#8292 = DIRECTION ( 'NONE',  ( -1.000000000000000000, 0.000000000000000000, 0.000000000000000000 ) ) ;
#8293 = UNCERTAINTY_MEASURE_WITH_UNIT (LENGTH_MEASURE( 1.000000000000000082E-05 ), #12067, 'distance_accuracy_value', 'NONE');
#8294 = ORIENTED_EDGE ( 'NONE', *, *, #8970, .F. ) ;
#8295 = CARTESIAN_POINT ( 'NONE',  ( 28.99095782554747913, 92.47818727009294548, -1.000000000000000000 ) ) ;
#8296 = DIRECTION ( 'NONE',  ( -1.000000000000000000, 0.000000000000000000, -0.000000000000000000 ) ) ;
#8297 = EDGE_LOOP ( 'NONE', ( #9106, #12647, #8134, #8635, #8548, #4699, #10062, #11298 ) ) ;
#8298 = DIRECTION ( 'NONE',  ( 0.000000000000000000, 0.000000000000000000, 1.000000000000000000 ) ) ;
#8299 = DIRECTION ( 'NONE',  ( 0.000000000000000000, 0.000000000000000000, 1.000000000000000000 ) ) ;
#8300 = EDGE_LOOP ( 'NONE', ( #135, #3623, #3659, #8743, #12692 ) ) ;
#8301 = AXIS2_PLACEMENT_3D ( 'NONE', #8994, #11020, #1811 ) ;
#8302 = ORIENTED_EDGE ( 'NONE', *, *, #4091, .T. ) ;
#8303 = ADVANCED_FACE ( 'NONE', ( #6865 ), #2196, .F. ) ;
#8304 = CARTESIAN_POINT ( 'NONE',  ( 0.000000000000000000, 27.00000000000000000, 0.000000000000000000 ) ) ;
#8305 = CARTESIAN_POINT ( 'NONE',  ( 1.040000000000000036, 1.154700538379252350, 7.017607234860990640E-28 ) ) ;
#8306 = VERTEX_POINT ( 'NONE', #8830 ) ;
#8307 = ORIENTED_EDGE ( 'NONE', *, *, #11838, .T. ) ;
#8308 = AXIS2_PLACEMENT_3D ( 'NONE', #10820, #10944, #10755 ) ;
#8309 = FACE_OUTER_BOUND ( 'NONE', #7164, .T. ) ;
#8310 = ORIENTED_EDGE ( 'NONE', *, *, #8901, .T. ) ;
#8311 = APPLICATION_PROTOCOL_DEFINITION ( 'draft international standard', 'automotive_design', 1998, #9009 ) ;
#8312 = CARTESIAN_POINT ( 'NONE',  ( 50.72178482187499071, 117.2309300971526937, 4.203125000614517326 ) ) ;
#8313 = EDGE_CURVE ( 'NONE', #362, #7384, #6801, .T. ) ;
#8314 = ORIENTED_EDGE ( 'NONE', *, *, #831, .F. ) ;
#8315 = FACE_OUTER_BOUND ( 'NONE', #5360, .T. ) ;
#8316 = EDGE_LOOP ( 'NONE', ( #12352, #5950, #12954, #3254, #12378 ) ) ;
#8317 = CARTESIAN_POINT ( 'NONE',  ( 34.25000000000000000, 93.41869858279433458, 6.000000000000000000 ) ) ;
#8318 = AXIS2_PLACEMENT_3D ( 'NONE', #1263, #5257, #9244 ) ;
#8319 = PLANE ( 'NONE',  #1720 ) ;
#8320 = DIRECTION ( 'NONE',  ( 0.000000000000000000, -1.000000000000000000, 0.000000000000000000 ) ) ;
#8321 = DIRECTION ( 'NONE',  ( -0.000000000000000000, -0.000000000000000000, -1.000000000000000000 ) ) ;
#8322 = ORIENTED_EDGE ( 'NONE', *, *, #10709, .F. ) ;
#8323 = CARTESIAN_POINT ( 'NONE',  ( 66.19999999999998863, 90.00000000000000000, 3.875000000000000000 ) ) ;
#8324 = ORIENTED_EDGE ( 'NONE', *, *, #2258, .T. ) ;
#8325 = AXIS2_PLACEMENT_3D ( 'NONE', #6116, #1144, #9263 ) ;
#8326 = EDGE_CURVE ( 'NONE', #11494, #12628, #925, .T. ) ;
#8327 = CARTESIAN_POINT ( 'NONE',  ( 1.040000000000000036, 0.5773502691896263972, 1.000000000000000000 ) ) ;
#8328 = VECTOR ( 'NONE', #4654, 1000.000000000000000 ) ;
#8329 = ORIENTED_EDGE ( 'NONE', *, *, #1489, .F. ) ;
#8330 = EDGE_CURVE ( 'NONE', #5069, #10466, #11594, .T. ) ;
#8331 = FACE_OUTER_BOUND ( 'NONE', #7001, .T. ) ;
#8332 = ORIENTED_EDGE ( 'NONE', *, *, #10275, .T. ) ;
#8333 = FACE_OUTER_BOUND ( 'NONE', #6079, .T. ) ;
#8334 = LINE ( 'NONE', #6295, #5357 ) ;
#8335 = CARTESIAN_POINT ( 'NONE',  ( 19.27821517812503060, 62.76906990284727783, 4.484375000614516438 ) ) ;
#8336 = CARTESIAN_POINT ( 'NONE',  ( -48.33333333333332860, -5.000000000000000000, -1.734723475976807094E-15 ) ) ;
#8337 = DIRECTION ( 'NONE',  ( 1.000000000000000000, 0.000000000000000000, 0.000000000000000000 ) ) ;
#8338 = CARTESIAN_POINT ( 'NONE',  ( 6.626776019045581556, 99.74475042915889844, -3.000000000000000000 ) ) ;
#8339 =( BOUNDED_CURVE ( )  B_SPLINE_CURVE ( 2, ( #10153, #8263, #12252, #5309, #9104, #3299, #11324 ),
 .UNSPECIFIED., .F., .F. ) 
 B_SPLINE_CURVE_WITH_KNOTS ( ( 3, 2, 2, 3 ),
 ( 0.8000000000000002665, 0.8333333333333334814, 0.8666666666666666963, 0.8885532418875740079 ),
 .UNSPECIFIED. ) 
 CURVE ( )  GEOMETRIC_REPRESENTATION_ITEM ( )  RATIONAL_B_SPLINE_CURVE ( ( 0.9999999999999991118, 0.8660254037844395958, 1.000000000000000000, 0.8660254037844387076, 1.000000000000000000, 0.9120326476671229976, 0.9395835397633002239 ) ) 
 REPRESENTATION_ITEM ( '' )  );
#8340 = PLANE ( 'NONE',  #6994 ) ;
#8341 = DIRECTION ( 'NONE',  ( 5.624500927088228034E-17, -1.370729058197317775E-18, -1.000000000000000000 ) ) ;
#8342 = LINE ( 'NONE', #2130, #9489 ) ;
#8343 = AXIS2_PLACEMENT_3D ( 'NONE', #9830, #9958, #796 ) ;
#8344 = DIRECTION ( 'NONE',  ( -1.000000000000000000, 0.000000000000000000, -0.000000000000000000 ) ) ;
#8345 = VECTOR ( 'NONE', #5836, 1000.000000000000114 ) ;
#8346 = DIRECTION ( 'NONE',  ( -0.000000000000000000, -0.000000000000000000, -1.000000000000000000 ) ) ;
#8347 = DIRECTION ( 'NONE',  ( -1.000000000000000000, 0.000000000000000000, -0.000000000000000000 ) ) ;
#8348 = EDGE_CURVE ( 'NONE', #6226, #10383, #7726, .T. ) ;
#8349 = ORIENTED_EDGE ( 'NONE', *, *, #2127, .F. ) ;
#8350 = DIRECTION ( 'NONE',  ( 0.000000000000000000, 1.000000000000000000, 0.000000000000000000 ) ) ;
#8351 = VERTEX_POINT ( 'NONE', #1966 ) ;
#8352 = PRODUCT ( 'conveyor wheel', 'conveyor wheel', '', ( #7260 ) ) ;
#8353 = CIRCLE ( 'NONE', #7518, 2.396199811936270407 ) ;
#8354 = CARTESIAN_POINT ( 'NONE',  ( 66.19999999999998863, 90.00000000000000000, 4.437500001229033764 ) ) ;
#8355 = CARTESIAN_POINT ( 'NONE',  ( 5.000000000000004441, 30.00000000000000000, 10.00000000000000000 ) ) ;
#8356 = CARTESIAN_POINT ( 'NONE',  ( 66.20000000000000284, 90.00000000000000000, 6.000000000000000000 ) ) ;
#8357 = EDGE_LOOP ( 'NONE', ( #6206, #5021, #3392, #8174, #3327, #3220, #6480, #6185 ) ) ;
#8358 = EDGE_CURVE ( 'NONE', #7336, #4743, #2889, .T. ) ;
#8359 = DIRECTION ( 'NONE',  ( 0.8660254037844361541, 0.5000000000000042188, 0.000000000000000000 ) ) ;
#8360 = CARTESIAN_POINT ( 'NONE',  ( 19.27821517812500574, 117.2309300971526937, 4.728125000614516793 ) ) ;
#8361 = ADVANCED_FACE ( 'NONE', ( #5882 ), #902, .T. ) ;
#8362 = VERTEX_POINT ( 'NONE', #1836 ) ;
#8363 = CIRCLE ( 'NONE', #400, 3.500000000000003109 ) ;
#8364 = DIRECTION ( 'NONE',  ( 0.000000000000000000, 0.000000000000000000, 1.000000000000000000 ) ) ;
#8365 = DIRECTION ( 'NONE',  ( 0.000000000000000000, 0.000000000000000000, 1.000000000000000000 ) ) ;
#8366 = EDGE_CURVE ( 'NONE', #12707, #4659, #4094, .T. ) ;
#8367 = EDGE_LOOP ( 'NONE', ( #6293, #5211, #88, #1372 ) ) ;
#8368 = VERTEX_POINT ( 'NONE', #9684 ) ;
#8369 = CARTESIAN_POINT ( 'NONE',  ( 2.387319993259524598, -4.036502139894371233, 0.000000000000000000 ) ) ;
#8370 = DIRECTION ( 'NONE',  ( 0.000000000000000000, 0.000000000000000000, 1.000000000000000000 ) ) ;
#8371 = VERTEX_POINT ( 'NONE', #9941 ) ;
#8372 = VECTOR ( 'NONE', #7569, 1000.000000000000000 ) ;
#8373 = AXIS2_PLACEMENT_3D ( 'NONE', #7485, #468, #2651 ) ;
#8374 = VERTEX_POINT ( 'NONE', #4782 ) ;
#8375 = CARTESIAN_POINT ( 'NONE',  ( 34.25000000000000000, 93.41869858279433458, -3.799999999999999378 ) ) ;
#8376 = VERTEX_POINT ( 'NONE', #12640 ) ;
#8377 = DIRECTION ( 'NONE',  ( 1.000000000000000000, 0.000000000000000000, 0.000000000000000000 ) ) ;
#8378 = ITEM_DEFINED_TRANSFORMATION ( 'NONE', 'NONE', #1541,  #5704 ) ;
#8379 = CARTESIAN_POINT ( 'NONE',  ( 66.20000000000000284, 71.98667160128370313, 3.050000001229034474 ) ) ;
#8380 = ADVANCED_FACE ( 'NONE', ( #8771 ), #9814, .T. ) ;
#8381 = ORIENTED_EDGE ( 'NONE', *, *, #8598, .F. ) ;
#8382 = DIRECTION ( 'NONE',  ( 0.000000000000000000, 0.000000000000000000, -1.000000000000000000 ) ) ;
#8383 = ORIENTED_EDGE ( 'NONE', *, *, #12077, .F. ) ;
#8384 = CIRCLE ( 'NONE', #7545, 1.500000000000001332 ) ;
#8385 = DIRECTION ( 'NONE',  ( 1.000000000000000000, 0.000000000000000000, 0.000000000000000000 ) ) ;
#8386 = LINE ( 'NONE', #4265, #448 ) ;
#8387 = DIRECTION ( 'NONE',  ( 1.000000000000000000, -0.000000000000000000, 0.000000000000000000 ) ) ;
#8388 = SURFACE_STYLE_FILL_AREA ( #10410 ) ;
#8389 = ORIENTED_EDGE ( 'NONE', *, *, #12796, .F. ) ;
#8390 = VECTOR ( 'NONE', #1586, 1000.000000000000000 ) ;
#8391 = CARTESIAN_POINT ( 'NONE',  ( 66.19999999999988916, 71.98667160128361786, 4.400000001229033231 ) ) ;
#8392 = CARTESIAN_POINT ( 'NONE',  ( -53.33333333333332149, 36.15840287135605990, -1.000000000000000000 ) ) ;
#8393 = EDGE_CURVE ( 'NONE', #1694, #29, #843, .T. ) ;
#8394 = CARTESIAN_POINT ( 'NONE',  ( 66.44356964374999563, 71.84604660189820891, 3.246875000614517059 ) ) ;
#8395 = ORIENTED_EDGE ( 'NONE', *, *, #7724, .T. ) ;
#8396 = ADVANCED_FACE ( 'NONE', ( #10668 ), #7917, .T. ) ;
#8397 = DIRECTION ( 'NONE',  ( 0.000000000000000000, 1.000000000000000000, 0.000000000000000000 ) ) ;
#8398 = CARTESIAN_POINT ( 'NONE',  ( 35.00000000000000000, 90.00000000000000000, 3.000000000000000000 ) ) ;
#8399 = CARTESIAN_POINT ( 'NONE',  ( 35.00000000000000000, 126.3079067962036106, 4.296875000614517326 ) ) ;
#8400 = EDGE_CURVE ( 'NONE', #4218, #6538, #7662, .T. ) ;
#8401 = DIRECTION ( 'NONE',  ( -0.000000000000000000, -0.000000000000000000, -1.000000000000000000 ) ) ;
#8402 = EDGE_CURVE ( 'NONE', #11615, #1698, #10727, .T. ) ;
#8403 = CARTESIAN_POINT ( 'NONE',  ( 33.50000000000000711, 67.79999999999999716, 8.000000000000000000 ) ) ;
#8404 = DIRECTION ( 'NONE',  ( 0.000000000000000000, -0.000000000000000000, 1.000000000000000000 ) ) ;
#8405 = DIRECTION ( 'NONE',  ( 0.000000000000000000, 0.000000000000000000, 1.000000000000000000 ) ) ;
#8406 = CARTESIAN_POINT ( 'NONE',  ( 35.00000000000000000, 90.00000000000000000, -0.9999999999999970024 ) ) ;
#8407=STYLED_ITEM('',(#12981),#12113);
#8408 = LINE ( 'NONE', #5651, #11183 ) ;
#8409 = DIRECTION ( 'NONE',  ( 0.000000000000000000, 0.000000000000000000, 1.000000000000000000 ) ) ;
#8410 = FACE_OUTER_BOUND ( 'NONE', #10191, .T. ) ;
#8411 = ORIENTED_EDGE ( 'NONE', *, *, #4326, .F. ) ;
#8412 = FACE_OUTER_BOUND ( 'NONE', #9474, .T. ) ;
#8413 = CARTESIAN_POINT ( 'NONE',  ( -1.436050757534458100, -5.516136167806656943, -0.8000000000000000444 ) ) ;
#8414 = VERTEX_POINT ( 'NONE', #4848 ) ;
#8415 = VECTOR ( 'NONE', #838, 1000.000000000000000 ) ;
#8416 = LINE ( 'NONE', #3452, #77 ) ;
#8417 = CARTESIAN_POINT ( 'NONE',  ( 1.040000000000000036, 0.000000000000000000, 0.000000000000000000 ) ) ;
#8418 = ADVANCED_FACE ( 'NONE', ( #6931, #42, #8242, #3146 ), #4126, .T. ) ;
#8419 = CARTESIAN_POINT ( 'NONE',  ( 66.19999999999998863, 90.00000000000000000, 3.087500001229034119 ) ) ;
#8420 = VERTEX_POINT ( 'NONE', #3213 ) ;
#8421 = CARTESIAN_POINT ( 'NONE',  ( 38.50000000000000711, 90.00000000000000000, 6.000000000000000000 ) ) ;
#8422 = DIRECTION ( 'NONE',  ( -1.000000000000000000, 0.000000000000000000, 0.000000000000000000 ) ) ;
#8423 = ORIENTED_EDGE ( 'NONE', *, *, #7323, .F. ) ;
#8424 =( NAMED_UNIT ( * ) PLANE_ANGLE_UNIT ( ) SI_UNIT ( $, .RADIAN. ) );
#8425 = LINE ( 'NONE', #9598, #11197 ) ;
#8426 = ORIENTED_EDGE ( 'NONE', *, *, #7806, .F. ) ;
#8427 = CARTESIAN_POINT ( 'NONE',  ( 50.00000000000000000, 2.000000000000000000, 10.00000000000000000 ) ) ;
#8428 = ORIENTED_EDGE ( 'NONE', *, *, #11483, .T. ) ;
#8429 = VECTOR ( 'NONE', #5864, 1000.000000000000000 ) ;
#8430 = CARTESIAN_POINT ( 'NONE',  ( 3.800000000000055334, 71.98667160128364628, 3.800000001229034474 ) ) ;
#8431 = PLANE ( 'NONE',  #1852 ) ;
#8432 = ORIENTED_EDGE ( 'NONE', *, *, #9603, .T. ) ;
#8433 = ADVANCED_FACE ( 'NONE', ( #111 ), #6075, .T. ) ;
#8434 = EDGE_LOOP ( 'NONE', ( #8069, #8592 ) ) ;
#8435 = LINE ( 'NONE', #10395, #10127 ) ;
#8436 = VERTEX_POINT ( 'NONE', #9149 ) ;
#8437 = AXIS2_PLACEMENT_3D ( 'NONE', #12560, #4704, #12684 ) ;
#8438 = CARTESIAN_POINT ( 'NONE',  ( 35.00000000000000000, 90.00000000000000000, -3.000000000000000000 ) ) ;
#8439 = PRODUCT_CONTEXT ( 'NONE', #8103, 'mechanical' ) ;
#8440 = CARTESIAN_POINT ( 'NONE',  ( 50.59999999999999432, 117.0199925980744666, 2.712500001229034119 ) ) ;
#8441 = ORIENTED_EDGE ( 'NONE', *, *, #9657, .F. ) ;
#8442 = LINE ( 'NONE', #12693, #11816 ) ;
#8443 = ORIENTED_EDGE ( 'NONE', *, *, #4228, .T. ) ;
#8444 = STYLED_ITEM ( 'NONE', ( #5468 ), #10270 ) ;
#8445 = PRESENTATION_STYLE_ASSIGNMENT (( #6602 ) ) ;
#8446 = ORIENTED_EDGE ( 'NONE', *, *, #4252, .T. ) ;
#8447 = DIRECTION ( 'NONE',  ( -1.000000000000000000, 0.000000000000000000, -0.000000000000000000 ) ) ;
#8448 = CARTESIAN_POINT ( 'NONE',  ( 35.75000000000000711, 92.49999999999998579, 4.000000000000000000 ) ) ;
#8449 = VECTOR ( 'NONE', #12200, 1000.000000000000000 ) ;
#8450 = EDGE_CURVE ( 'NONE', #6664, #4357, #7191, .T. ) ;
#8451 = AXIS2_PLACEMENT_3D ( 'NONE', #10178, #1214, #4237 ) ;
#8452 = ORIENTED_EDGE ( 'NONE', *, *, #6150, .T. ) ;
#8453 = CARTESIAN_POINT ( 'NONE',  ( 3.556430356250014579, 108.1539533981018053, 3.471875000614516704 ) ) ;
#8454 = ORIENTED_EDGE ( 'NONE', *, *, #1233, .F. ) ;
#8455 = CARTESIAN_POINT ( 'NONE',  ( 3.800000000000015365, 90.00000000000000000, 3.312500001229034652 ) ) ;
#8456 = EDGE_LOOP ( 'NONE', ( #5157, #10345, #965, #6462 ) ) ;
#8457 = AXIS2_PLACEMENT_3D ( 'NONE', #9, #6832, #6772 ) ;
#8458 = CARTESIAN_POINT ( 'NONE',  ( 3.556430356250015024, 90.00000000000000000, 3.059375000614517059 ) ) ;
#8459 = PRODUCT ( 'sorter block', 'sorter block', '', ( #2619 ) ) ;
#8460 = ORIENTED_EDGE ( 'NONE', *, *, #3785, .F. ) ;
#8461 = VECTOR ( 'NONE', #6560, 1000.000000000000000 ) ;
#8462 = CARTESIAN_POINT ( 'NONE',  ( 35.00000000000000000, 90.00000000000000000, 5.000000000000000000 ) ) ;
#8463 = DIRECTION ( 'NONE',  ( 0.000000000000000000, 0.000000000000000000, 1.000000000000000000 ) ) ;
#8464 = CARTESIAN_POINT ( 'NONE',  ( 3.556430356250028790, 71.84604660189818048, 4.446875000614517681 ) ) ;
#8465 = DIRECTION ( 'NONE',  ( 0.000000000000000000, 0.000000000000000000, 1.000000000000000000 ) ) ;
#8466 = ADVANCED_FACE ( 'NONE', ( #8113 ), #2297, .F. ) ;
#8467 = CYLINDRICAL_SURFACE ( 'NONE', #379, 31.19999999999999929 ) ;
#8468 = AXIS2_PLACEMENT_3D ( 'NONE', #5450, #2778, #1856 ) ;
#8469 = CARTESIAN_POINT ( 'NONE',  ( 3.800000000000015365, 90.00000000000000000, 3.650000000000000355 ) ) ;
#8470 = CARTESIAN_POINT ( 'NONE',  ( -23.49999999999998934, 51.07328482542158810, -1.000000000000000000 ) ) ;
#8471 = DIRECTION ( 'NONE',  ( -0.9549484348006340717, -0.2967717757331703732, 0.000000000000000000 ) ) ;
#8472 = DIRECTION ( 'NONE',  ( -0.3262398754384822630, 0.9452870165584014162, 0.000000000000000000 ) ) ;
#8473 = FACE_OUTER_BOUND ( 'NONE', #11176, .T. ) ;
#8474 = EDGE_CURVE ( 'NONE', #5822, #294, #5536, .T. ) ;
#8475 = DIRECTION ( 'NONE',  ( 0.000000000000000000, 0.000000000000000000, 1.000000000000000000 ) ) ;
#8476 = AXIS2_PLACEMENT_3D ( 'NONE', #1084, #10902, #8817 ) ;
#8477 = CARTESIAN_POINT ( 'NONE',  ( 7.500000000000000000, 30.00000000000000000, -1.499999999999999556 ) ) ;
#8478 = VERTEX_POINT ( 'NONE', #9214 ) ;
#8479=STYLED_ITEM('',(#13016),#3242);
#8480 = DIRECTION ( 'NONE',  ( 0.000000000000000000, 0.000000000000000000, 1.000000000000000000 ) ) ;
#8481 = DIRECTION ( 'NONE',  ( 1.000000000000000000, 0.000000000000000000, -0.000000000000000000 ) ) ;
#8482 = VERTEX_POINT ( 'NONE', #7126 ) ;
#8483 = EDGE_CURVE ( 'NONE', #10249, #10977, #3012, .T. ) ;
#8484 = CARTESIAN_POINT ( 'NONE',  ( 30.00000000000000711, 0.000000000000000000, 10.00000000000000000 ) ) ;
#8485 = CARTESIAN_POINT ( 'NONE',  ( 3.800000000000039790, 71.98667160128364628, 4.587500000000000355 ) ) ;
#8486 = AXIS2_PLACEMENT_3D ( 'NONE', #538, #2584, #3636 ) ;
#8487 = CARTESIAN_POINT ( 'NONE',  ( 25.00000000000000355, -5.000000000000000000, -7.250000000000000888 ) ) ;
#8488 = AXIS2_PLACEMENT_3D ( 'NONE', #491, #7570, #4436 ) ;
#8489 = ORIENTED_EDGE ( 'NONE', *, *, #3741, .T. ) ;
#8490 = CARTESIAN_POINT ( 'NONE',  ( 25.00000000000000355, 0.000000000000000000, -4.249999999999998224 ) ) ;
#8491 = CARTESIAN_POINT ( 'NONE',  ( 35.00000000000000711, 53.69209320379639649, 4.465625000614517504 ) ) ;
#8492 = ADVANCED_FACE ( 'NONE', ( #6134 ), #10979, .T. ) ;
#8493 = ORIENTED_EDGE ( 'NONE', *, *, #4395, .F. ) ;
#8494 = CARTESIAN_POINT ( 'NONE',  ( 0.000000000000000000, 0.000000000000000000, 0.000000000000000000 ) ) ;
#8495 = DIRECTION ( 'NONE',  ( -1.000000000000000000, 0.000000000000000000, 0.000000000000000000 ) ) ;
#8496 = VERTEX_POINT ( 'NONE', #11966 ) ;
#8497 = LINE ( 'NONE', #6454, #1824 ) ;
#8498 = ORIENTED_EDGE ( 'NONE', *, *, #10591, .F. ) ;
#8499 = VECTOR ( 'NONE', #8039, 1000.000000000000000 ) ;
#8500 = LINE ( 'NONE', #10455, #5900 ) ;
#8501 = CARTESIAN_POINT ( 'NONE',  ( 35.75000000000000711, 93.41869858279433458, 6.000000000000000000 ) ) ;
#8502 = ORIENTED_EDGE ( 'NONE', *, *, #200, .T. ) ;
#8503 = ORIENTED_EDGE ( 'NONE', *, *, #9390, .F. ) ;
#8504 = DIRECTION ( 'NONE',  ( 0.000000000000000000, 0.000000000000000000, 1.000000000000000000 ) ) ;
#8505 = ORIENTED_EDGE ( 'NONE', *, *, #11585, .F. ) ;
#8506 = DIRECTION ( 'NONE',  ( -0.000000000000000000, -0.000000000000000000, -1.000000000000000000 ) ) ;
#8507 = CARTESIAN_POINT ( 'NONE',  ( 35.00000000000000711, 53.97334320256736362, 3.875000001229034208 ) ) ;
#8508 = VECTOR ( 'NONE', #6838, 1000.000000000000000 ) ;
#8509 = ORIENTED_EDGE ( 'NONE', *, *, #8758, .F. ) ;
#8510 = SURFACE_SIDE_STYLE ('',( #2687 ) ) ;
#8511 = VERTEX_POINT ( 'NONE', #10004 ) ;
#8512 = PRESENTATION_STYLE_ASSIGNMENT (( #5560 ) ) ;
#8513 = ORIENTED_EDGE ( 'NONE', *, *, #11633, .F. ) ;
#8514 = EDGE_CURVE ( 'NONE', #1636, #10706, #3046, .T. ) ;
#8515 = CARTESIAN_POINT ( 'NONE',  ( 20.04920293992519831, 62.48814478912512982, 3.000000000000001776 ) ) ;
#8516 = CARTESIAN_POINT ( 'NONE',  ( -57.99999999999999289, 30.00000000000000000, -8.000000000000005329 ) ) ;
#8517 = VECTOR ( 'NONE', #10737, 1000.000000000000000 ) ;
#8518 = ORIENTED_EDGE ( 'NONE', *, *, #4557, .T. ) ;
#8519 = LINE ( 'NONE', #4460, #7825 ) ;
#8520 = EDGE_LOOP ( 'NONE', ( #8921, #4946, #2285, #1970 ) ) ;
#8521 = CARTESIAN_POINT ( 'NONE',  ( 66.19999999999988916, 71.98667160128361786, 3.050000001229034030 ) ) ;
#8522 = ORIENTED_EDGE ( 'NONE', *, *, #7789, .F. ) ;
#8523 = DIRECTION ( 'NONE',  ( -0.000000000000000000, 0.000000000000000000, -1.000000000000000000 ) ) ;
#8524 = VERTEX_POINT ( 'NONE', #6273 ) ;
#8525 = EDGE_CURVE ( 'NONE', #10542, #9930, #4297, .T. ) ;
#8526 = ADVANCED_FACE ( 'NONE', ( #8176 ), #11177, .F. ) ;
#8527 = AXIS2_PLACEMENT_3D ( 'NONE', #1324, #9047, #12130 ) ;
#8528 = CARTESIAN_POINT ( 'NONE',  ( 72.83557806687970526, 62.54593364529978317, 1.000000000000003109 ) ) ;
#8529 = CARTESIAN_POINT ( 'NONE',  ( 10.10814115972632088, 109.2382489648782240, 3.000000000000001332 ) ) ;
#8530 = EDGE_CURVE ( 'NONE', #1585, #10599, #10352, .T. ) ;
#8531 = CARTESIAN_POINT ( 'NONE',  ( 35.00000000000000000, 90.00000000000000000, -3.000000000000000000 ) ) ;
#8532 = CARTESIAN_POINT ( 'NONE',  ( 3.556430356250014579, 108.1539533981018053, 4.315625000614517148 ) ) ;
#8533 = APPLICATION_CONTEXT ( 'automotive_design' ) ;
#8534 = CARTESIAN_POINT ( 'NONE',  ( 4.800000000000015810, 90.00000000000000000, 5.000000000000000000 ) ) ;
#8535 = CARTESIAN_POINT ( 'NONE',  ( 49.99999999999996447, 90.00000000000000000, -5.000000000000000000 ) ) ;
#8536 = CIRCLE ( 'NONE', #6227, 28.99999999999999289 ) ;
#8537 = AXIS2_PLACEMENT_3D ( 'NONE', #11055, #12177, #1110 ) ;
#8538 = LINE ( 'NONE', #6495, #7625 ) ;
#8539 = CARTESIAN_POINT ( 'NONE',  ( 52.49999999999996447, 86.00000000000000000, -10.00000000000000000 ) ) ;
#8540 = LINE ( 'NONE', #9641, #3234 ) ;
#8541 = DIRECTION ( 'NONE',  ( 0.000000000000000000, 0.000000000000000000, 1.000000000000000000 ) ) ;
#8542 = EDGE_CURVE ( 'NONE', #4807, #3419, #8957, .T. ) ;
#8543 = CARTESIAN_POINT ( 'NONE',  ( -60.00000000000000000, 30.00000000000000000, 3.000000000000000000 ) ) ;
#8544 = FACE_OUTER_BOUND ( 'NONE', #12375, .T. ) ;
#8545 = VERTEX_POINT ( 'NONE', #2232 ) ;
#8546 = CARTESIAN_POINT ( 'NONE',  ( 5.000000000000004441, 30.00000000000000000, 2.500000000000000444 ) ) ;
#8547 = DIRECTION ( 'NONE',  ( 0.4719909656437444867, -0.8816033849473842166, 0.000000000000000000 ) ) ;
#8548 = ORIENTED_EDGE ( 'NONE', *, *, #6843, .F. ) ;
#8549 = CARTESIAN_POINT ( 'NONE',  ( 45.00000000000000000, 3.649999999999993694, -5.750000000000000000 ) ) ;
#8550 = CARTESIAN_POINT ( 'NONE',  ( 4.999999999999962697, 79.07477288111861924, -3.000000000000000000 ) ) ;
#8551 = CARTESIAN_POINT ( 'NONE',  ( 35.00000000000000000, 90.00000000000000000, -10.00000000000000000 ) ) ;
#8552 = DIRECTION ( 'NONE',  ( 0.000000000000000000, -0.000000000000000000, -1.000000000000000000 ) ) ;
#8553 = AXIS2_PLACEMENT_3D ( 'NONE', #1129, #11074, #3112 ) ;
#8554 = ORIENTED_EDGE ( 'NONE', *, *, #10833, .F. ) ;
#8555 = LINE ( 'NONE', #12545, #10764 ) ;
#8556 = DIRECTION ( 'NONE',  ( -1.000000000000000000, 0.000000000000000000, 0.000000000000000000 ) ) ;
#8557 = EDGE_CURVE ( 'NONE', #12599, #11555, #2421, .T. ) ;
#8558 = EDGE_LOOP ( 'NONE', ( #10479, #1039, #10251, #4256 ) ) ;
#8559 = DIRECTION ( 'NONE',  ( 0.000000000000000000, 0.000000000000000000, -1.000000000000000000 ) ) ;
#8560 = CARTESIAN_POINT ( 'NONE',  ( 22.99999999999998579, 90.00000000000000000, -5.000000000000000000 ) ) ;
#8561 = VERTEX_POINT ( 'NONE', #10129 ) ;
#8562 = CIRCLE ( 'NONE', #4802, 1.599999999999990319 ) ;
#8563 = DIRECTION ( 'NONE',  ( -0.000000000000000000, -0.000000000000000000, -1.000000000000000000 ) ) ;
#8564 = EDGE_LOOP ( 'NONE', ( #7894, #3446, #5367, #11394, #1384 ) ) ;
#8565 = AXIS2_PLACEMENT_3D ( 'NONE', #1183, #4269, #8257 ) ;
#8566 = DIRECTION ( 'NONE',  ( -1.000000000000000000, -0.000000000000000000, -0.000000000000000000 ) ) ;
#8567 = CARTESIAN_POINT ( 'NONE',  ( 5.000000000000004441, 30.00000000000000000, -2.500000000000000000 ) ) ;
#8568 = EDGE_CURVE ( 'NONE', #8022, #454, #94, .T. ) ;
#8569 = EDGE_CURVE ( 'NONE', #3419, #9344, #5159, .T. ) ;
#8570 = CARTESIAN_POINT ( 'NONE',  ( 0.000000000000000000, 3.490243377569955568E-16, -2.849999999999999201 ) ) ;
#8571 = VERTEX_POINT ( 'NONE', #11502 ) ;
#8573 = DIRECTION ( 'NONE',  ( -1.000000000000000000, 0.000000000000000000, -0.000000000000000000 ) ) ;
#8572 = VECTOR ( 'NONE', #8884, 1000.000000000000000 ) ;
#8574 = ORIENTED_EDGE ( 'NONE', *, *, #7830, .F. ) ;
#8575 = FACE_OUTER_BOUND ( 'NONE', #7313, .T. ) ;
#8576 = CARTESIAN_POINT ( 'NONE',  ( 3.800000000000015365, 108.0133283987163111, 4.175000001229034474 ) ) ;
#8577 = ORIENTED_EDGE ( 'NONE', *, *, #7590, .T. ) ;
#8578 = ORIENTED_EDGE ( 'NONE', *, *, #97, .T. ) ;
#8579 = ORIENTED_EDGE ( 'NONE', *, *, #10942, .T. ) ;
#8580 = CARTESIAN_POINT ( 'NONE',  ( 10.32967766089132233, 70.63732739706711072, 3.000000000000001776 ) ) ;
#8581 = CIRCLE ( 'NONE', #7318, 1.500000000000000222 ) ;
#8582 = PLANE ( 'NONE',  #358 ) ;
#8583 = UNCERTAINTY_MEASURE_WITH_UNIT (LENGTH_MEASURE( 1.000000000000000082E-05 ), #7431, 'distance_accuracy_value', 'NONE');
#8584 = PRODUCT_DEFINITION ( 'UNKNOWN', '', #8658, #12872 ) ;
#8585 = VERTEX_POINT ( 'NONE', #4512 ) ;
#8586 = CARTESIAN_POINT ( 'NONE',  ( 3.556430356250015024, 90.00000000000000000, 3.959375000614517415 ) ) ;
#8587 = EDGE_LOOP ( 'NONE', ( #9734, #8195, #3189 ) ) ;
#8588 = EDGE_CURVE ( 'NONE', #11707, #7918, #4446, .T. ) ;
#8589 = PLANE ( 'NONE',  #4381 ) ;
#8590 = ORIENTED_EDGE ( 'NONE', *, *, #5202, .F. ) ;
#8591 = CARTESIAN_POINT ( 'NONE',  ( 66.44356964374998142, 108.1539533981018053, 4.221875000614517148 ) ) ;
#8592 = ORIENTED_EDGE ( 'NONE', *, *, #2094, .F. ) ;
#8593 = CARTESIAN_POINT ( 'NONE',  ( 1.000000000000000000, -4.873461295629625489, 0.000000000000000000 ) ) ;
#8594 = CARTESIAN_POINT ( 'NONE',  ( 12.79502542898369555, 112.2861453170762474, 2.999999999999998224 ) ) ;
#8595 = DIRECTION ( 'NONE',  ( 0.000000000000000000, 0.000000000000000000, 1.000000000000000000 ) ) ;
#8596 = CARTESIAN_POINT ( 'NONE',  ( -60.00000000000000000, 30.00000000000000000, -2.500000000000000000 ) ) ;
#8597 = AXIS2_PLACEMENT_3D ( 'NONE', #1730, #4740, #10751 ) ;
#8598 = EDGE_CURVE ( 'NONE', #309, #3927, #7519, .T. ) ;
#8599 = CARTESIAN_POINT ( 'NONE',  ( 1.000000000000000000, -5.473461295629626022, -0.8000000000000000444 ) ) ;
#8600 = PLANE ( 'NONE',  #12423 ) ;
#8601 = ADVANCED_FACE ( 'NONE', ( #3472 ), #11569, .F. ) ;
#8602 = CARTESIAN_POINT ( 'NONE',  ( 7.577945032559769700, 99.43561875886716450, 3.000000000000001332 ) ) ;
#8603 = DIRECTION ( 'NONE',  ( 0.000000000000000000, -0.000000000000000000, 1.000000000000000000 ) ) ;
#8604 = CARTESIAN_POINT ( 'NONE',  ( -2.387319993259524598, -4.036502139894371233, -0.8000000000000000444 ) ) ;
#8605 = VECTOR ( 'NONE', #2434, 1000.000000000000114 ) ;
#8606 = CARTESIAN_POINT ( 'NONE',  ( 3.800000000000015365, 90.00000000000000000, 3.650000000000000355 ) ) ;
#8607 = DIRECTION ( 'NONE',  ( 0.9347165045408831752, 0.3553942263724512163, 0.000000000000000000 ) ) ;
#8608 = VERTEX_POINT ( 'NONE', #7321 ) ;
#8609 = DIRECTION ( 'NONE',  ( -5.624500927088228034E-17, 1.370729058197317775E-18, 1.000000000000000000 ) ) ;
#8610 = EDGE_LOOP ( 'NONE', ( #7579, #12098, #12887, #160 ) ) ;
#8611 = EDGE_CURVE ( 'NONE', #6279, #11952, #7428, .T. ) ;
#8612 = LINE ( 'NONE', #3646, #2607 ) ;
#8613 = DIRECTION ( 'NONE',  ( -0.000000000000000000, -0.000000000000000000, -1.000000000000000000 ) ) ;
#8614 = ORIENTED_EDGE ( 'NONE', *, *, #5011, .F. ) ;
#8615 = CARTESIAN_POINT ( 'NONE',  ( 6.500000000000005329, 68.39379290111055809, 3.000000000000038636 ) ) ;
#8616 = CARTESIAN_POINT ( 'NONE',  ( 50.72178482187499071, 117.2309300971526937, 4.203125000614517326 ) ) ;
#8617 = VERTEX_POINT ( 'NONE', #11370 ) ;
#8618 = LINE ( 'NONE', #12797, #12133 ) ;
#8619 = CARTESIAN_POINT ( 'NONE',  ( 48.49999999999995737, 90.00000000000000000, -10.00000000000000178 ) ) ;
#8620 = ORIENTED_EDGE ( 'NONE', *, *, #9902, .F. ) ;
#8621 = AXIS2_PLACEMENT_3D ( 'NONE', #9097, #981, #12835 ) ;
#8622 = CARTESIAN_POINT ( 'NONE',  ( 3.800000000000015365, 90.00000000000000000, 4.549999999999999822 ) ) ;
#8623 = ORIENTED_EDGE ( 'NONE', *, *, #12906, .T. ) ;
#8624 = DIRECTION ( 'NONE',  ( -1.000000000000000000, 0.000000000000000000, 0.000000000000000000 ) ) ;
#8625 = DIRECTION ( 'NONE',  ( -0.000000000000000000, -0.000000000000000000, -1.000000000000000000 ) ) ;
#8626 = EDGE_CURVE ( 'NONE', #9403, #7451, #7835, .T. ) ;
#8627 = DIRECTION ( 'NONE',  ( 0.8660254037844361541, 0.5000000000000042188, -9.389466242107225456E-17 ) ) ;
#8628 = DIRECTION ( 'NONE',  ( -1.000000000000000000, -0.000000000000000000, -0.000000000000000000 ) ) ;
#8629 = VECTOR ( 'NONE', #8043, 1000.000000000000000 ) ;
#8630 = CARTESIAN_POINT ( 'NONE',  ( 9.999999999999994671, 70.41451884327426569, 2.500000000000000444 ) ) ;
#8631 = VERTEX_POINT ( 'NONE', #8375 ) ;
#8632 = DIRECTION ( 'NONE',  ( -0.000000000000000000, -1.000000000000000000, -0.000000000000000000 ) ) ;
#8633 = PRODUCT_CONTEXT ( 'NONE', #2515, 'mechanical' ) ;
#8634 = CARTESIAN_POINT ( 'NONE',  ( 66.19999999999998863, 90.00000000000000000, 3.087500001229034119 ) ) ;
#8635 = ORIENTED_EDGE ( 'NONE', *, *, #11951, .F. ) ;
#8636 = DIRECTION ( 'NONE',  ( 0.000000000000000000, 0.5000000000000003331, 0.8660254037844383745 ) ) ;
#8637 = EDGE_CURVE ( 'NONE', #11833, #12128, #734, .T. ) ;
#8638 = EDGE_LOOP ( 'NONE', ( #802, #6155, #9150, #10658 ) ) ;
#8639 = EDGE_CURVE ( 'NONE', #9191, #4447, #6331, .T. ) ;
#8640 = VERTEX_POINT ( 'NONE', #11437 ) ;
#8641 = DIRECTION ( 'NONE',  ( -1.000000000000000000, 0.000000000000000000, -0.000000000000000000 ) ) ;
#8642 = COLOUR_RGB ( '',0.8941176470588234615, 0.8941176470588234615, 0.8941176470588234615 ) ;
#8643 = DIRECTION ( 'NONE',  ( -0.000000000000000000, -1.000000000000000000, -0.000000000000000000 ) ) ;
#8644 = AXIS2_PLACEMENT_3D ( 'NONE', #9894, #67, #11128 ) ;
#8645 = EDGE_CURVE ( 'NONE', #11848, #8056, #1364, .T. ) ;
#8646 = EDGE_LOOP ( 'NONE', ( #10614, #9395, #2289, #9111 ) ) ;
#8647 = DIRECTION ( 'NONE',  ( -1.000000000000000000, -0.000000000000000000, -0.000000000000000000 ) ) ;
#8648 = ORIENTED_EDGE ( 'NONE', *, *, #6736, .F. ) ;
#8649 = CARTESIAN_POINT ( 'NONE',  ( 45.00000000000000000, -5.000000000000000000, 4.249999999999999112 ) ) ;
#8650 = ORIENTED_EDGE ( 'NONE', *, *, #11181, .F. ) ;
#8651 = CARTESIAN_POINT ( 'NONE',  ( 66.44356964374999563, 71.84604660189820891, 4.596875000614517148 ) ) ;
#8652 = ORIENTED_EDGE ( 'NONE', *, *, #1437, .T. ) ;
#8653 = DIRECTION ( 'NONE',  ( 0.000000000000000000, 1.000000000000000000, 0.000000000000000000 ) ) ;
#8654 = CLOSED_SHELL ( 'NONE', ( #3977, #1466, #11868, #8752, #1092, #2040, #5839, #4796, #6860, #7829, #2998, #5194, #2498, #12616, #7910, #7903, #11350, #8361, #8657, #3766, #2766, #8687, #12922, #2168, #6518, #7468 ) ) ;
#8655 = LINE ( 'NONE', #11658, #5789 ) ;
#8656 = CARTESIAN_POINT ( 'NONE',  ( 3.556430356250014579, 108.1539533981018053, 3.865625000614517415 ) ) ;
#8657 = ADVANCED_FACE ( 'NONE', ( #8309 ), #2357, .T. ) ;
#8658 = PRODUCT_DEFINITION_FORMATION_WITH_SPECIFIED_SOURCE ( 'ANY', '', #4489, .NOT_KNOWN. ) ;
#8659 = DIRECTION ( 'NONE',  ( -1.000000000000000000, 0.000000000000000000, 0.000000000000000000 ) ) ;
#8660 = CARTESIAN_POINT ( 'NONE',  ( 50.60000000000001563, 62.98000740192552627, 3.912500001229034297 ) ) ;
#8661 = CARTESIAN_POINT ( 'NONE',  ( 25.00000000000000355, -5.000000000000000000, -5.750000000000000000 ) ) ;
#8662 = CARTESIAN_POINT ( 'NONE',  ( 45.00000000000000711, 90.00000000000000000, -18.00000000000000355 ) ) ;
#8663 = VECTOR ( 'NONE', #5976, 1000.000000000000000 ) ;
#8664 = DIRECTION ( 'NONE',  ( 0.000000000000000000, -1.000000000000000000, 0.000000000000000000 ) ) ;
#8665 = DIRECTION ( 'NONE',  ( 0.000000000000000000, 0.000000000000000000, -1.000000000000000000 ) ) ;
#8666 = CARTESIAN_POINT ( 'NONE',  ( 66.44356964374998142, 108.1539533981018053, 4.221875000614517148 ) ) ;
#8667 = ORIENTED_EDGE ( 'NONE', *, *, #10848, .F. ) ;
#8668 = CARTESIAN_POINT ( 'NONE',  ( 19.40000000000002700, 62.98000740192551206, 3.275000000000000355 ) ) ;
#8669 = CARTESIAN_POINT ( 'NONE',  ( 3.800000000000015365, 90.00000000000000000, 5.000000000000000000 ) ) ;
#8670 = EDGE_LOOP ( 'NONE', ( #9596, #1060, #2442, #12686 ) ) ;
#8671 = AXIS2_PLACEMENT_3D ( 'NONE', #12119, #12053, #8377 ) ;
#8672 = EDGE_CURVE ( 'NONE', #4270, #3017, #6464, .T. ) ;
#8673 = SURFACE_SIDE_STYLE ('',( #4490 ) ) ;
#8674 = AXIS2_PLACEMENT_3D ( 'NONE', #665, #1462, #3503 ) ;
#8675 = FACE_OUTER_BOUND ( 'NONE', #6122, .T. ) ;
#8676 = DIRECTION ( 'NONE',  ( 0.000000000000000000, 0.000000000000000000, 1.000000000000000000 ) ) ;
#8677 = VECTOR ( 'NONE', #12020, 1000.000000000000000 ) ;
#8678 = CARTESIAN_POINT ( 'NONE',  ( -60.00000000000000000, 30.00000000000000000, -0.9999999999999991118 ) ) ;
#8679 = CARTESIAN_POINT ( 'NONE',  ( 3.556430356250015024, 90.00000000000000000, 3.003125000614517148 ) ) ;
#8680 = AXIS2_PLACEMENT_3D ( 'NONE', #780, #8895, #3936 ) ;
#8681 = DIRECTION ( 'NONE',  ( 0.000000000000000000, 0.000000000000000000, 1.000000000000000000 ) ) ;
#8682 = DIRECTION ( 'NONE',  ( 0.000000000000000000, 0.000000000000000000, -1.000000000000000000 ) ) ;
#8683 = EDGE_LOOP ( 'NONE', ( #8243, #6535 ) ) ;
#8684 = EDGE_CURVE ( 'NONE', #12608, #4194, #9410, .T. ) ;
#8685 = CARTESIAN_POINT ( 'NONE',  ( 35.00000000000000000, 126.0266567974326222, 4.437500000000000888 ) ) ;
#8686 = ORIENTED_EDGE ( 'NONE', *, *, #11061, .T. ) ;
#8687 = ADVANCED_FACE ( 'NONE', ( #5416 ), #7383, .T. ) ;
#8688 = CARTESIAN_POINT ( 'NONE',  ( 33.50000000000000711, 67.79999999999999716, 6.000000000000000000 ) ) ;
#8689 = CYLINDRICAL_SURFACE ( 'NONE', #7912, 31.19999999999998863 ) ;
#8690 = AXIS2_PLACEMENT_3D ( 'NONE', #2268, #7096, #144 ) ;
#8691 = COLOUR_RGB ( '',0.8941176470588234615, 0.8941176470588234615, 0.8941176470588234615 ) ;
#8692 = CARTESIAN_POINT ( 'NONE',  ( -60.00000000000000000, 30.00000000000000000, 9.999999999999996447 ) ) ;
#8693 = ORIENTED_EDGE ( 'NONE', *, *, #6306, .F. ) ;
#8694 = CARTESIAN_POINT ( 'NONE',  ( 0.000000000000000000, 0.000000000000000000, 1.000000000000000000 ) ) ;
#8695 = EDGE_LOOP ( 'NONE', ( #4570, #213, #1303, #5113 ) ) ;
#8696 = CARTESIAN_POINT ( 'NONE',  ( 25.00000000000000355, 2.000000000000000000, -4.150000000000007461 ) ) ;
#8697 = CARTESIAN_POINT ( 'NONE',  ( 17.66025403784438197, 77.14656965084323303, -1.000000000000000000 ) ) ;
#8698 = EDGE_LOOP ( 'NONE', ( #2624, #10635, #8038, #4375 ) ) ;
#8699 = CARTESIAN_POINT ( 'NONE',  ( 35.00000000000000000, 90.00000000000000000, 6.000000000000000000 ) ) ;
#8700 = EDGE_LOOP ( 'NONE', ( #7568, #11112, #6673, #4248 ) ) ;
#8701 = EDGE_CURVE ( 'NONE', #8368, #7529, #8435, .T. ) ;
#8702 = ORIENTED_EDGE ( 'NONE', *, *, #8982, .T. ) ;
#8703 = CARTESIAN_POINT ( 'NONE',  ( 7.180262550876764571, 75.42990296268297357, 3.000000000000000444 ) ) ;
#8704 = DIRECTION ( 'NONE',  ( 1.000000000000000000, 0.000000000000000000, 5.337610695313252124E-17 ) ) ;
#8706 = EDGE_CURVE ( 'NONE', #7837, #12083, #9093, .T. ) ;
#8705 = ORIENTED_EDGE ( 'NONE', *, *, #8483, .T. ) ;
#8707 = VECTOR ( 'NONE', #728, 1000.000000000000000 ) ;
#8708 = DIRECTION ( 'NONE',  ( 0.000000000000000000, 0.000000000000000000, 1.000000000000000000 ) ) ;
#8709 = VERTEX_POINT ( 'NONE', #7452 ) ;
#8710 = PLANE ( 'NONE',  #3974 ) ;
#8711 = EDGE_LOOP ( 'NONE', ( #2641, #4179, #5703, #1168 ) ) ;
#8712 = CARTESIAN_POINT ( 'NONE',  ( 50.72178482187499071, 117.2309300971526937, 2.853125000614517237 ) ) ;
#8713 = ORIENTED_EDGE ( 'NONE', *, *, #4432, .F. ) ;
#8714 = DIRECTION ( 'NONE',  ( -5.624500927088228034E-17, 1.370729058197317775E-18, 1.000000000000000000 ) ) ;
#8715 = CARTESIAN_POINT ( 'NONE',  ( 66.20000000000004547, 108.0133283987162969, 3.912500000000000977 ) ) ;
#8716 = AXIS2_PLACEMENT_3D ( 'NONE', #5203, #1336, #9126 ) ;
#8717 =( NAMED_UNIT ( * ) SI_UNIT ( $, .STERADIAN. ) SOLID_ANGLE_UNIT ( ) );
#8718 = CARTESIAN_POINT ( 'NONE',  ( 66.44356964374999563, 71.84604660189820891, 3.640625000614517326 ) ) ;
#8719 = LINE ( 'NONE', #3948, #810 ) ;
#8720 = EDGE_CURVE ( 'NONE', #2378, #5783, #8880, .T. ) ;
#8721 = ADVANCED_FACE ( 'NONE', ( #7581 ), #5480, .T. ) ;
#8722 = DIRECTION ( 'NONE',  ( -1.000000000000000000, 0.000000000000000000, -0.000000000000000000 ) ) ;
#8723 = CARTESIAN_POINT ( 'NONE',  ( 45.00000000000000000, -5.000000000000000000, -4.249999999999998224 ) ) ;
#8724 = FACE_OUTER_BOUND ( 'NONE', #8695, .T. ) ;
#8725 = CIRCLE ( 'NONE', #9769, 6.450000000000001066 ) ;
#8726 = DIRECTION ( 'NONE',  ( 1.000000000000000000, 0.000000000000000000, 0.000000000000000000 ) ) ;
#8727 = DIRECTION ( 'NONE',  ( -0.000000000000000000, 1.000000000000000000, -0.000000000000000000 ) ) ;
#8728 = CARTESIAN_POINT ( 'NONE',  ( 3.556430356250014579, 108.1539533981018053, 3.021875000614517415 ) ) ;
#8729 = ORIENTED_EDGE ( 'NONE', *, *, #7590, .F. ) ;
#8730 = CARTESIAN_POINT ( 'NONE',  ( 3.800000000000015365, 108.0133283987163111, 4.062500000000000000 ) ) ;
#8731 = CARTESIAN_POINT ( 'NONE',  ( 31.80092274341787828, 89.00581455129388075, 4.800000000000000711 ) ) ;
#8732 = ORIENTED_EDGE ( 'NONE', *, *, #6752, .T. ) ;
#8733 = AXIS2_PLACEMENT_3D ( 'NONE', #382, #8387, #10471 ) ;
#8734 = DIRECTION ( 'NONE',  ( 0.000000000000000000, -1.000000000000000000, 0.000000000000000000 ) ) ;
#8735 = CARTESIAN_POINT ( 'NONE',  ( 35.00000000000000000, 90.00000000000000000, 1.000000000000003553 ) ) ;
#8736 = CARTESIAN_POINT ( 'NONE',  ( -60.00000000000000000, 30.00000000000000000, 3.000000000000000000 ) ) ;
#8737 = CARTESIAN_POINT ( 'NONE',  ( 3.000000000000004441, 27.00000000000000000, 2.500000000000000000 ) ) ;
#8738 = ADVANCED_FACE ( 'NONE', ( #12806 ), #4831, .T. ) ;
#8739 = CARTESIAN_POINT ( 'NONE',  ( 50.72178482187499071, 117.2309300971526937, 3.303125000614517415 ) ) ;
#8740 = VECTOR ( 'NONE', #10259, 1000.000000000000000 ) ;
#8741 = LINE ( 'NONE', #876, #3155 ) ;
#8742 = CARTESIAN_POINT ( 'NONE',  ( 50.72178482187499071, 117.2309300971526937, 4.259375000614517681 ) ) ;
#8743 = ORIENTED_EDGE ( 'NONE', *, *, #632, .T. ) ;
#8744 = LINE ( 'NONE', #4947, #5158 ) ;
#8745 = EDGE_LOOP ( 'NONE', ( #1903, #10085, #178, #8849 ) ) ;
#8746 = DIRECTION ( 'NONE',  ( -1.000000000000000000, -0.000000000000000000, -0.000000000000000000 ) ) ;
#8747 = FACE_OUTER_BOUND ( 'NONE', #9421, .T. ) ;
#8748 = CIRCLE ( 'NONE', #6446, 10.00000000000000178 ) ;
#8749 = CARTESIAN_POINT ( 'NONE',  ( 25.00000000000000355, 0.000000000000000000, -7.250000000000000888 ) ) ;
#8751 = EDGE_CURVE ( 'NONE', #12799, #9156, #4499, .T. ) ;
#8750 = DIRECTION ( 'NONE',  ( -0.8660254037844361541, -0.5000000000000042188, 9.389466242107221759E-17 ) ) ;
#8752 = ADVANCED_FACE ( 'NONE', ( #11761 ), #6656, .T. ) ;
#8753 = CARTESIAN_POINT ( 'NONE',  ( 1.040000000000000036, -1.154700538379251240, 1.014316938424154191E-17 ) ) ;
#8754 =( BOUNDED_CURVE ( )  B_SPLINE_CURVE ( 2, ( #3490, #8521, #2701, #7470, #12510, #11455, #7664 ),
 .UNSPECIFIED., .F., .F. ) 
 B_SPLINE_CURVE_WITH_KNOTS ( ( 3, 2, 2, 3 ),
 ( 0.7000000000000001776, 0.7333333333333335036, 0.7666666666666669405, 0.8000000000000002665 ),
 .UNSPECIFIED. ) 
 CURVE ( )  GEOMETRIC_REPRESENTATION_ITEM ( )  RATIONAL_B_SPLINE_CURVE ( ( 0.9999999999999991118, 0.8660254037844395958, 1.000000000000000000, 0.8660254037844387076, 1.000000000000000000, 0.8660254037844378194, 1.000000000000000888 ) ) 
 REPRESENTATION_ITEM ( '' )  );
#8755 = CARTESIAN_POINT ( 'NONE',  ( 35.00000000000000000, 90.00000000000000000, 1.500000000000000888 ) ) ;
#8756 = ORIENTED_EDGE ( 'NONE', *, *, #5082, .F. ) ;
#8757 = LINE ( 'NONE', #1695, #1137 ) ;
#8758 = EDGE_CURVE ( 'NONE', #8640, #7938, #7215, .T. ) ;
#8759 = CONTEXT_DEPENDENT_SHAPE_REPRESENTATION ( #4517, #5233 ) ;
#8760 = DIRECTION ( 'NONE',  ( 1.000000000000000000, 0.000000000000000000, 0.000000000000000000 ) ) ;
#8761 = EDGE_LOOP ( 'NONE', ( #12582, #2609, #346, #10667 ) ) ;
#8762 = AXIS2_PLACEMENT_3D ( 'NONE', #5649, #3633, #8471 ) ;
#8763 = ORIENTED_EDGE ( 'NONE', *, *, #12712, .F. ) ;
#8764 = CONICAL_SURFACE ( 'NONE', #5632, 1.500000000000001332, 1.029744260000000633 ) ;
#8765 = ORIENTED_EDGE ( 'NONE', *, *, #10673, .F. ) ;
#8766 = CARTESIAN_POINT ( 'NONE',  ( 42.94697885295607165, 59.81164240722340963, 2.999999999999999112 ) ) ;
#8767 = DIRECTION ( 'NONE',  ( 0.000000000000000000, 0.000000000000000000, 1.000000000000000000 ) ) ;
#8768 = VECTOR ( 'NONE', #7870, 1000.000000000000000 ) ;
#8769 = ADVANCED_FACE ( 'NONE', ( #8815 ), #10594, .T. ) ;
#8770 = VERTEX_POINT ( 'NONE', #7645 ) ;
#8771 = FACE_OUTER_BOUND ( 'NONE', #10694, .T. ) ;
#8772 = EDGE_LOOP ( 'NONE', ( #5226, #12094, #5868, #5081, #10339 ) ) ;
#8773 =( REPRESENTATION_RELATIONSHIP ('NONE','NONE', #1997, #9014 ) REPRESENTATION_RELATIONSHIP_WITH_TRANSFORMATION ( #5419 )SHAPE_REPRESENTATION_RELATIONSHIP( ) );
#8774 = CARTESIAN_POINT ( 'NONE',  ( 21.49999999999998579, 90.00000000000000000, -8.000000000000000000 ) ) ;
#8775 = ORIENTED_EDGE ( 'NONE', *, *, #9402, .T. ) ;
#8776 = CARTESIAN_POINT ( 'NONE',  ( 19.27821517812503060, 62.76906990284727783, 3.978125000614516793 ) ) ;
#8777 = ORIENTED_EDGE ( 'NONE', *, *, #2114, .T. ) ;
#8778 = AXIS2_PLACEMENT_3D ( 'NONE', #11358, #2410, #8556 ) ;
#8779 = DIRECTION ( 'NONE',  ( -0.000000000000000000, -0.000000000000000000, -1.000000000000000000 ) ) ;
#8780 = DIRECTION ( 'NONE',  ( 0.000000000000000000, 0.000000000000000000, -1.000000000000000000 ) ) ;
#8781 = CARTESIAN_POINT ( 'NONE',  ( 50.72178482187499071, 117.2309300971526937, 3.753125000614517592 ) ) ;
#8782 = CARTESIAN_POINT ( 'NONE',  ( 1.269999999999999796, 0.000000000000000000, 0.000000000000000000 ) ) ;
#8783 = ADVANCED_FACE ( 'NONE', ( #9798, #12685 ), #766, .T. ) ;
#8784 = CARTESIAN_POINT ( 'NONE',  ( 19.40000000000002700, 62.98000740192551206, 4.287500001229034297 ) ) ;
#8785 = AXIS2_PLACEMENT_3D ( 'NONE', #1934, #1007, #5005 ) ;
#8786 = DIRECTION ( 'NONE',  ( 1.000000000000000000, 0.000000000000000000, 0.000000000000000000 ) ) ;
#8787 = CARTESIAN_POINT ( 'NONE',  ( 50.00000000000000000, 62.64236852357281293, 5.000000000000000000 ) ) ;
#8788 = DIRECTION ( 'NONE',  ( -0.000000000000000000, 0.4999999999999998890, -0.8660254037844387076 ) ) ;
#8789 = CARTESIAN_POINT ( 'NONE',  ( -23.49999999999999289, 51.07328482542158810, 1.000000000000000000 ) ) ;
#8790 = DIRECTION ( 'NONE',  ( -0.000000000000000000, -0.5000000000000003331, 0.8660254037844384856 ) ) ;
#8791 = DIRECTION ( 'NONE',  ( -1.000000000000000000, 0.000000000000000000, 0.000000000000000000 ) ) ;
#8793 = EDGE_CURVE ( 'NONE', #7791, #1672, #5676, .T. ) ;
#8792 = ORIENTED_EDGE ( 'NONE', *, *, #8557, .T. ) ;
#8794 = ADVANCED_FACE ( 'NONE', ( #2936 ), #11828, .F. ) ;
#8795 =( NAMED_UNIT ( * ) PLANE_ANGLE_UNIT ( ) SI_UNIT ( $, .RADIAN. ) );
#8796 = VECTOR ( 'NONE', #1124, 1000.000000000000000 ) ;
#8797 = CARTESIAN_POINT ( 'NONE',  ( 21.49999999999998579, 90.00000000000000000, -8.000000000000000000 ) ) ;
#8798 = ORIENTED_EDGE ( 'NONE', *, *, #4286, .F. ) ;
#8799 = LINE ( 'NONE', #10947, #11154 ) ;
#8800 = CARTESIAN_POINT ( 'NONE',  ( 52.44898870156725224, 66.83414752204051013, -1.000000000000000222 ) ) ;
#8801 = CIRCLE ( 'NONE', #3176, 1.599999999999999645 ) ;
#8802 = CARTESIAN_POINT ( 'NONE',  ( 64.31840976852106451, 100.6710284717588024, 2.999476386674974737 ) ) ;
#8803 = CARTESIAN_POINT ( 'NONE',  ( 50.72178482187499071, 117.2309300971526937, 3.753125000614517592 ) ) ;
#8804 = DIRECTION ( 'NONE',  ( 1.000000000000000000, 0.000000000000000000, 0.000000000000000000 ) ) ;
#8805 = CARTESIAN_POINT ( 'NONE',  ( 35.00000000000000000, 126.3079067962036106, 3.846875000614517592 ) ) ;
#8806 = ORIENTED_EDGE ( 'NONE', *, *, #34, .T. ) ;
#8807 = DIRECTION ( 'NONE',  ( 0.000000000000000000, 0.000000000000000000, -1.000000000000000000 ) ) ;
#8808 = VERTEX_POINT ( 'NONE', #5617 ) ;
#8809 = COLOUR_RGB ( '',0.8941176470588234615, 0.8941176470588234615, 0.8941176470588234615 ) ;
#8810 = DIRECTION ( 'NONE',  ( -0.000000000000000000, 1.000000000000000000, -0.000000000000000000 ) ) ;
#8811 = EDGE_CURVE ( 'NONE', #9386, #10351, #2874, .T. ) ;
#8812 = LINE ( 'NONE', #12012, #6642 ) ;
#8813 = DIRECTION ( 'NONE',  ( 0.000000000000000000, 0.000000000000000000, -1.000000000000000000 ) ) ;
#8814 = LINE ( 'NONE', #10899, #12820 ) ;
#8815 = FACE_OUTER_BOUND ( 'NONE', #4051, .T. ) ;
#8816 = ORIENTED_EDGE ( 'NONE', *, *, #11102, .T. ) ;
#8817 = DIRECTION ( 'NONE',  ( 1.000000000000000000, 0.000000000000000000, 0.000000000000000000 ) ) ;
#8818 = CARTESIAN_POINT ( 'NONE',  ( 1.040000000000000036, 0.000000000000000000, 1.000000000000000000 ) ) ;
#8819 = ORIENTED_EDGE ( 'NONE', *, *, #1171, .F. ) ;
#8820 = VECTOR ( 'NONE', #597, 1000.000000000000000 ) ;
#8821 = ORIENTED_EDGE ( 'NONE', *, *, #11796, .T. ) ;
#8822 = EDGE_CURVE ( 'NONE', #7638, #3214, #8881, .T. ) ;
#8823 = PRESENTATION_STYLE_ASSIGNMENT (( #8041 ) ) ;
#8824 = VERTEX_POINT ( 'NONE', #8630 ) ;
#8825 = CARTESIAN_POINT ( 'NONE',  ( 0.000000000000000000, 0.000000000000000000, 0.000000000000000000 ) ) ;
#8826 = CARTESIAN_POINT ( 'NONE',  ( 9.999999999999994671, 30.00000000000000000, 2.500000000000000444 ) ) ;
#8827 = EDGE_CURVE ( 'NONE', #3168, #4495, #3667, .T. ) ;
#8828 = AXIS2_PLACEMENT_3D ( 'NONE', #6715, #8566, #4505 ) ;
#8829 = ORIENTED_EDGE ( 'NONE', *, *, #5751, .F. ) ;
#8830 = CARTESIAN_POINT ( 'NONE',  ( 9.136132550659251450, 74.79933025939541835, 1.000000000000003553 ) ) ;
#8831 = ORIENTED_EDGE ( 'NONE', *, *, #419, .F. ) ;
#8832 = CARTESIAN_POINT ( 'NONE',  ( 4.999999999999962697, 79.07477288111861924, 1.000000000000000000 ) ) ;
#8833 = ORIENTED_EDGE ( 'NONE', *, *, #5921, .F. ) ;
#8834 = CARTESIAN_POINT ( 'NONE',  ( 35.00000000000000711, 53.69209320379640360, 3.565625000614517592 ) ) ;
#8835 = ORIENTED_EDGE ( 'NONE', *, *, #1100, .T. ) ;
#8836 = STYLED_ITEM ( 'NONE', ( #11348 ), #10604 ) ;
#8837 = DIRECTION ( 'NONE',  ( -1.000000000000000000, 0.000000000000000000, 0.000000000000000000 ) ) ;
#8838 = DIRECTION ( 'NONE',  ( -0.000000000000000000, 1.000000000000000000, -0.000000000000000000 ) ) ;
#8839 = EDGE_CURVE ( 'NONE', #2101, #12533, #10665, .T. ) ;
#8840 = CARTESIAN_POINT ( 'NONE',  ( 66.19999999999998863, 90.00000000000000000, 4.774999999999999467 ) ) ;
#8841 = CARTESIAN_POINT ( 'NONE',  ( 19.27821517812500574, 117.2309300971526937, 4.278125000614516615 ) ) ;
#8842 = VECTOR ( 'NONE', #7898, 999.9999999999998863 ) ;
#8843 = ADVANCED_FACE ( 'NONE', ( #4706 ), #3727, .F. ) ;
#8844 = DIRECTION ( 'NONE',  ( -0.000000000000000000, -1.000000000000000000, -0.000000000000000000 ) ) ;
#8845 = ORIENTED_EDGE ( 'NONE', *, *, #7758, .T. ) ;
#8846 = LINE ( 'NONE', #1854, #1987 ) ;
#8847 = LINE ( 'NONE', #8787, #2709 ) ;
#8848 = DIRECTION ( 'NONE',  ( 0.000000000000000000, 0.000000000000000000, 1.000000000000000000 ) ) ;
#8849 = ORIENTED_EDGE ( 'NONE', *, *, #2532, .F. ) ;
#8850 = VECTOR ( 'NONE', #3195, 1000.000000000000000 ) ;
#8851 = DIRECTION ( 'NONE',  ( -0.000000000000000000, 0.000000000000000000, 1.000000000000000000 ) ) ;
#8852 = EDGE_LOOP ( 'NONE', ( #1226, #3681, #2558, #10550, #11165, #7502, #10009, #10451 ) ) ;
#8853 = DIRECTION ( 'NONE',  ( 0.03100775193798452692, -0.9995191440486532741, 0.000000000000000000 ) ) ;
#8854 = CARTESIAN_POINT ( 'NONE',  ( 66.44356964374999563, 71.84604660189820891, 4.146875000614517859 ) ) ;
#8855 = ORIENTED_EDGE ( 'NONE', *, *, #11067, .F. ) ;
#8856 = EDGE_CURVE ( 'NONE', #6452, #2378, #12876, .T. ) ;
#8858 = CARTESIAN_POINT ( 'NONE',  ( 19.40000000000000924, 117.0199925980744666, 3.575000000000000178 ) ) ;
#8857 = AXIS2_PLACEMENT_3D ( 'NONE', #8549, #4685, #1474 ) ;
#8859 = CARTESIAN_POINT ( 'NONE',  ( 45.00000000000000000, 2.000000000000000000, 5.750000000000000888 ) ) ;
#8860 = ORIENTED_EDGE ( 'NONE', *, *, #539, .F. ) ;
#8861 = AXIS2_PLACEMENT_3D ( 'NONE', #2522, #469, #9513 ) ;
#8862 = AXIS2_PLACEMENT_3D ( 'NONE', #12732, #8013, #12791 ) ;
#8863 = DIRECTION ( 'NONE',  ( -0.5000000000000043299, 0.8660254037844362651, 0.000000000000000000 ) ) ;
#8864 = CARTESIAN_POINT ( 'NONE',  ( 7.266925300896119211, 98.48530999652632545, 4.000000000000000000 ) ) ;
#8865 = EDGE_CURVE ( 'NONE', #11250, #4553, #3790, .T. ) ;
#8866 = DIRECTION ( 'NONE',  ( 0.8660254037844361541, 0.5000000000000042188, 0.000000000000000000 ) ) ;
#8867 = CARTESIAN_POINT ( 'NONE',  ( 4.999999999999962697, 79.07477288111861924, 3.000000000000000000 ) ) ;
#8868 = CIRCLE ( 'NONE', #290, 3.350000000000000089 ) ;
#8869 = FACE_OUTER_BOUND ( 'NONE', #4121, .T. ) ;
#8870 = ORIENTED_EDGE ( 'NONE', *, *, #4803, .T. ) ;
#8871 = AXIS2_PLACEMENT_3D ( 'NONE', #8972, #1916, #10872 ) ;
#8872 = CYLINDRICAL_SURFACE ( 'NONE', #8301, 28.99999999999999289 ) ;
#8873 = VERTEX_POINT ( 'NONE', #5808 ) ;
#8874 =( NAMED_UNIT ( * ) PLANE_ANGLE_UNIT ( ) SI_UNIT ( $, .RADIAN. ) );
#8875 = CARTESIAN_POINT ( 'NONE',  ( 16.96438320935645905, 66.02675393316422969, 1.000000000000003109 ) ) ;
#8876 = LINE ( 'NONE', #5013, #7168 ) ;
#8877 = CIRCLE ( 'NONE', #6373, 0.7499999999999997780 ) ;
#8878 = CARTESIAN_POINT ( 'NONE',  ( 1.040000000000000036, 0.000000000000000000, 2.000000000000000000 ) ) ;
#8879 = EDGE_CURVE ( 'NONE', #3957, #2378, #12760, .T. ) ;
#8880 = CIRCLE ( 'NONE', #12856, 3.500000000000003109 ) ;
#8881 = LINE ( 'NONE', #1693, #12731 ) ;
#8882 = ORIENTED_EDGE ( 'NONE', *, *, #11025, .T. ) ;
#8883 = DIRECTION ( 'NONE',  ( 0.000000000000000000, 0.000000000000000000, 1.000000000000000000 ) ) ;
#8884 = DIRECTION ( 'NONE',  ( -0.000000000000000000, -0.000000000000000000, -1.000000000000000000 ) ) ;
#8885 = ORIENTED_EDGE ( 'NONE', *, *, #5347, .F. ) ;
#8886 = DIRECTION ( 'NONE',  ( 0.000000000000000000, 0.000000000000000000, 1.000000000000000000 ) ) ;
#8887 = EDGE_LOOP ( 'NONE', ( #2831, #2953, #12877, #10841 ) ) ;
#8888 = SURFACE_STYLE_FILL_AREA ( #5752 ) ;
#8890 = ORIENTED_EDGE ( 'NONE', *, *, #7379, .T. ) ;
#8889 = CIRCLE ( 'NONE', #6803, 1.599999999999986766 ) ;
#8891 = VECTOR ( 'NONE', #10720, 1000.000000000000114 ) ;
#8892 = CARTESIAN_POINT ( 'NONE',  ( 8.499999999999998224, 71.85789451624832225, -1.000000000000000222 ) ) ;
#8893 = CARTESIAN_POINT ( 'NONE',  ( -60.00000000000000000, 23.99999999999998934, 2.500000000000000000 ) ) ;
#8894 = EDGE_LOOP ( 'NONE', ( #2865, #5696 ) ) ;
#8895 = DIRECTION ( 'NONE',  ( -0.000000000000000000, -0.000000000000000000, -1.000000000000000000 ) ) ;
#8896 = EDGE_LOOP ( 'NONE', ( #7081, #1365, #7646, #6742 ) ) ;
#8897 = VECTOR ( 'NONE', #10814, 1000.000000000000114 ) ;
#8898 = CARTESIAN_POINT ( 'NONE',  ( 35.00000000000000000, 90.00000000000000000, 6.000000000000000000 ) ) ;
#8899 = ORIENTED_EDGE ( 'NONE', *, *, #9983, .T. ) ;
#8900 = FACE_BOUND ( 'NONE', #7140, .T. ) ;
#8901 = EDGE_CURVE ( 'NONE', #10113, #1516, #8276, .T. ) ;
#8902 = EDGE_LOOP ( 'NONE', ( #6859, #11244, #2154, #8454 ) ) ;
#8903 = DIRECTION ( 'NONE',  ( 0.000000000000000000, 0.000000000000000000, -1.000000000000000000 ) ) ;
#8904 = CARTESIAN_POINT ( 'NONE',  ( 17.54971918633085437, 66.83239978927272773, 4.000000000000000000 ) ) ;
#8905 = DIRECTION ( 'NONE',  ( 0.000000000000000000, 0.000000000000000000, 1.000000000000000000 ) ) ;
#8906 = CARTESIAN_POINT ( 'NONE',  ( 66.44356964374998142, 108.1539533981018053, 3.715625000614517948 ) ) ;
#8907 = CARTESIAN_POINT ( 'NONE',  ( 1.040000000000000036, 1.154700538379252350, 7.017607234860990640E-28 ) ) ;
#8908 = VERTEX_POINT ( 'NONE', #6302 ) ;
#8909 = CARTESIAN_POINT ( 'NONE',  ( 0.1325741768533959530, -4.273461295629625845, 0.000000000000000000 ) ) ;
#8910 = EDGE_CURVE ( 'NONE', #8371, #12624, #4350, .T. ) ;
#8911 = EDGE_CURVE ( 'NONE', #12578, #12915, #11142, .T. ) ;
#8912 = DIRECTION ( 'NONE',  ( -0.000000000000000000, 1.000000000000000000, -0.000000000000000000 ) ) ;
#8913 = DIRECTION ( 'NONE',  ( 0.000000000000000000, 0.000000000000000000, 1.000000000000000000 ) ) ;
#8914 = VERTEX_POINT ( 'NONE', #10365 ) ;
#8915 = DIRECTION ( 'NONE',  ( -0.000000000000000000, 0.000000000000000000, 1.000000000000000000 ) ) ;
#8916 = ADVANCED_FACE ( 'NONE', ( #11278 ), #1268, .F. ) ;
#8917 = ORIENTED_EDGE ( 'NONE', *, *, #12833, .T. ) ;
#8918 = AXIS2_PLACEMENT_3D ( 'NONE', #3465, #2738, #5473 ) ;
#8919 = DIRECTION ( 'NONE',  ( 0.000000000000000000, 0.000000000000000000, 1.000000000000000000 ) ) ;
#8920 = FACE_OUTER_BOUND ( 'NONE', #4840, .T. ) ;
#8921 = ORIENTED_EDGE ( 'NONE', *, *, #12153, .F. ) ;
#8922 = CARTESIAN_POINT ( 'NONE',  ( 19.27821517812500574, 117.2309300971526937, 4.784375000614516260 ) ) ;
#8923 = DIRECTION ( 'NONE',  ( -1.000000000000000000, 0.000000000000000000, 0.000000000000000000 ) ) ;
#8924 = AXIS2_PLACEMENT_3D ( 'NONE', #8797, #933, #8923 ) ;
#8925 = CARTESIAN_POINT ( 'NONE',  ( 8.499999999999992895, 69.54849343948981755, 3.000000000000000000 ) ) ;
#8926 = ADVANCED_FACE ( 'NONE', ( #6106 ), #10295, .T. ) ;
#8927 = CARTESIAN_POINT ( 'NONE',  ( 35.75000000000000711, 93.50000000000000000, -4.802775637732004554 ) ) ;
#8928 = FACE_OUTER_BOUND ( 'NONE', #3353, .T. ) ;
#8929 = DIRECTION ( 'NONE',  ( 0.000000000000000000, 0.000000000000000000, 1.000000000000000000 ) ) ;
#8930 = CARTESIAN_POINT ( 'NONE',  ( -53.33333333333332149, 79.07477288111861924, -1.000000000000000000 ) ) ;
#8931 = ORIENTED_EDGE ( 'NONE', *, *, #5314, .T. ) ;
#8932 = AXIS2_PLACEMENT_3D ( 'NONE', #11449, #4456, #2437 ) ;
#8933 = LINE ( 'NONE', #3782, #12267 ) ;
#8934 = ORIENTED_EDGE ( 'NONE', *, *, #9832, .T. ) ;
#8935 = CARTESIAN_POINT ( 'NONE',  ( 50.00000000000000000, 0.000000000000000000, -10.00000000000000000 ) ) ;
#8936 = CARTESIAN_POINT ( 'NONE',  ( 2.300000000000003375, 90.00000000000000000, 6.000000000000000000 ) ) ;
#8937 = CARTESIAN_POINT ( 'NONE',  ( 4.270088556250601699E-16, 2.000000000000000000, -8.000000000000000000 ) ) ;
#8938 = EDGE_CURVE ( 'NONE', #2627, #3833, #1328, .T. ) ;
#8939 = CARTESIAN_POINT ( 'NONE',  ( 45.00000000000000000, 2.000000000000000000, -7.349999999999993427 ) ) ;
#8940 = VECTOR ( 'NONE', #9748, 1000.000000000000000 ) ;
#8941 = ORIENTED_EDGE ( 'NONE', *, *, #3607, .T. ) ;
#8942 = DIRECTION ( 'NONE',  ( 0.000000000000000000, 0.000000000000000000, -1.000000000000000000 ) ) ;
#8943 = LINE ( 'NONE', #3670, #10448 ) ;
#8944 = ORIENTED_EDGE ( 'NONE', *, *, #3350, .T. ) ;
#8945 = CARTESIAN_POINT ( 'NONE',  ( 45.00000000000000000, -5.000000000000000000, 5.750000000000000888 ) ) ;
#8946 = ORIENTED_EDGE ( 'NONE', *, *, #12642, .F. ) ;
#8947 = DIRECTION ( 'NONE',  ( -1.084202172485504064E-16, 0.000000000000000000, -1.000000000000000000 ) ) ;
#8948 = ORIENTED_EDGE ( 'NONE', *, *, #7361, .F. ) ;
#8949 = EDGE_CURVE ( 'NONE', #11492, #10844, #7715, .T. ) ;
#8950 = AXIS2_PLACEMENT_3D ( 'NONE', #4762, #2611, #7704 ) ;
#8951 = EDGE_CURVE ( 'NONE', #8561, #1735, #2074, .T. ) ;
#8952 = DIRECTION ( 'NONE',  ( -0.000000000000000000, -0.000000000000000000, -1.000000000000000000 ) ) ;
#8953 = CARTESIAN_POINT ( 'NONE',  ( 8.923698042205888470, 69.79311561821251075, 2.500000000000000444 ) ) ;
#8954 = ORIENTED_EDGE ( 'NONE', *, *, #7097, .T. ) ;
#8955 = EDGE_LOOP ( 'NONE', ( #3749, #1126, #5947, #706, #6527, #11704 ) ) ;
#8957 = LINE ( 'NONE', #11108, #2628 ) ;
#8956 = AXIS2_PLACEMENT_3D ( 'NONE', #7678, #3504, #11666 ) ;
#8958 = ORIENTED_EDGE ( 'NONE', *, *, #3206, .F. ) ;
#8959 = LINE ( 'NONE', #2827, #12110 ) ;
#8960 = ORIENTED_EDGE ( 'NONE', *, *, #2802, .T. ) ;
#8961 = CARTESIAN_POINT ( 'NONE',  ( 66.44356964374998142, 108.1539533981018053, 4.165625000614516793 ) ) ;
#8962 = ORIENTED_EDGE ( 'NONE', *, *, #6268, .F. ) ;
#8963 = CARTESIAN_POINT ( 'NONE',  ( 62.73309762663101452, 98.48529854432332797, 1.000000000000003109 ) ) ;
#8964 = CARTESIAN_POINT ( 'NONE',  ( 7.500000000000000000, 27.00000000000000000, 1.599999999999986766 ) ) ;
#8965 = CARTESIAN_POINT ( 'NONE',  ( 35.00000000000000711, 53.97334320256736362, 3.425000001229034474 ) ) ;
#8966 = VECTOR ( 'NONE', #3166, 1000.000000000000000 ) ;
#8967 = CARTESIAN_POINT ( 'NONE',  ( 3.800000000000015365, 108.0133283987163111, 3.725000001229034297 ) ) ;
#8968 = VECTOR ( 'NONE', #5139, 1000.000000000000000 ) ;
#8969 = FACE_OUTER_BOUND ( 'NONE', #6668, .T. ) ;
#8970 = EDGE_CURVE ( 'NONE', #36, #5609, #9249, .T. ) ;
#8971 = VERTEX_POINT ( 'NONE', #10900 ) ;
#8972 = CARTESIAN_POINT ( 'NONE',  ( 1.040000000000000036, 0.000000000000000000, 0.000000000000000000 ) ) ;
#8973 = CARTESIAN_POINT ( 'NONE',  ( 1.617350269189632428, 0.000000000000000000, 0.000000000000000000 ) ) ;
#8974 = CARTESIAN_POINT ( 'NONE',  ( 3.800000000000004707, 90.00000000000000000, 6.000000000000000000 ) ) ;
#8975 = ORIENTED_EDGE ( 'NONE', *, *, #4903, .T. ) ;
#8976 = DIRECTION ( 'NONE',  ( 0.000000000000000000, 0.000000000000000000, -1.000000000000000000 ) ) ;
#8977 = VERTEX_POINT ( 'NONE', #340 ) ;
#8978 = CARTESIAN_POINT ( 'NONE',  ( 1.040000000000000036, -1.154700538379251684, 0.000000000000000000 ) ) ;
#8979 = CARTESIAN_POINT ( 'NONE',  ( 3.556430356250028790, 71.84604660189818048, 3.490625000614517415 ) ) ;
#8980 = VERTEX_POINT ( 'NONE', #5195 ) ;
#8981 = CARTESIAN_POINT ( 'NONE',  ( 66.44356964374999563, 90.00000000000000000, 3.734375000614516882 ) ) ;
#8982 = EDGE_CURVE ( 'NONE', #5937, #9364, #5323, .T. ) ;
#8983 = CARTESIAN_POINT ( 'NONE',  ( 20.00000000000000355, 2.000000000000001776, -1.499999999999999556 ) ) ;
#8984 = PRODUCT_DEFINITION_SHAPE ( 'NONE', 'NONE',  #12961 ) ;
#8985 = VECTOR ( 'NONE', #9384, 1000.000000000000114 ) ;
#8986 = EDGE_CURVE ( 'NONE', #216, #4697, #4992, .T. ) ;
#8987 = DIRECTION ( 'NONE',  ( -0.000000000000000000, 0.000000000000000000, 1.000000000000000000 ) ) ;
#8988 = PLANE ( 'NONE',  #11786 ) ;
#8989 = FACE_OUTER_BOUND ( 'NONE', #4632, .T. ) ;
#8990 = CONICAL_SURFACE ( 'NONE', #1904, 1.500000000000001332, 1.029744260000000411 ) ;
#8991 = CARTESIAN_POINT ( 'NONE',  ( 4.338286831716297698, 0.4117131682837005258, -0.8000000000000000444 ) ) ;
#8992 = CARTESIAN_POINT ( 'NONE',  ( 6.499999999999998224, 65.10243346208218895, 1.000000000000000000 ) ) ;
#8993 = ORIENTED_EDGE ( 'NONE', *, *, #3565, .T. ) ;
#8994 = CARTESIAN_POINT ( 'NONE',  ( 35.00000000000000000, 90.00000000000000000, 4.000000000000000000 ) ) ;
#8995 = ORIENTED_EDGE ( 'NONE', *, *, #1200, .T. ) ;
#8996 = ADVANCED_FACE ( 'NONE', ( #12329 ), #3378, .F. ) ;
#8997 = CARTESIAN_POINT ( 'NONE',  ( 0.000000000000000000, 0.000000000000000000, 0.000000000000000000 ) ) ;
#8998 = CIRCLE ( 'NONE', #4418, 6.499999999999999112 ) ;
#8999 = LINE ( 'NONE', #23, #10823 ) ;
#9000 = PLANE ( 'NONE',  #9261 ) ;
#9001 = LINE ( 'NONE', #8939, #11774 ) ;
#9002 = EDGE_LOOP ( 'NONE', ( #12897, #10912 ) ) ;
#9003 = DIRECTION ( 'NONE',  ( 0.000000000000000000, 0.000000000000000000, 1.000000000000000000 ) ) ;
#9004 = DIRECTION ( 'NONE',  ( -0.000000000000000000, 1.000000000000000000, -0.000000000000000000 ) ) ;
#9005 = EDGE_LOOP ( 'NONE', ( #2824, #3398, #7247, #436 ) ) ;
#9006 = CARTESIAN_POINT ( 'NONE',  ( 35.75000000000000711, 92.49999999999998579, -8.000000000000000000 ) ) ;
#9007 = ORIENTED_EDGE ( 'NONE', *, *, #9115, .F. ) ;
#9008 = AXIS2_PLACEMENT_3D ( 'NONE', #964, #2463, #12090 ) ;
#9009 = APPLICATION_CONTEXT ( 'automotive_design' ) ;
#9010 = CARTESIAN_POINT ( 'NONE',  ( 40.00000000000000000, 0.000000000000000000, 10.00000000000000000 ) ) ;
#9011 = ORIENTED_EDGE ( 'NONE', *, *, #9639, .F. ) ;
#9012 = EDGE_CURVE ( 'NONE', #865, #2507, #1044, .T. ) ;
#9013 = CARTESIAN_POINT ( 'NONE',  ( 31.80092274341787828, 89.00581455129388075, 4.000000000000000000 ) ) ;
#9014 = SHAPE_REPRESENTATION ( 'circlip for shafts normal_din_Circlip DIN 471 - 7 x 0.8', ( #5704 ), #1107 ) ;
#9015 = LINE ( 'NONE', #38, #9785 ) ;
#9016 = ADVANCED_BREP_SHAPE_REPRESENTATION ( '', ( #7850, #5704 ), #2789 ) ;
#9017 = ORIENTED_EDGE ( 'NONE', *, *, #9162, .F. ) ;
#9018 = VERTEX_POINT ( 'NONE', #6174 ) ;
#9019 = VECTOR ( 'NONE', #121, 1000.000000000000000 ) ;
#9020 = CARTESIAN_POINT ( 'NONE',  ( 45.00000000000000000, 2.000000000000001332, 5.750000000000000888 ) ) ;
#9021 = VERTEX_POINT ( 'NONE', #3313 ) ;
#9022 = ADVANCED_FACE ( 'NONE', ( #10166 ), #9184, .F. ) ;
#9023 = CARTESIAN_POINT ( 'NONE',  ( 50.72178482187499071, 117.2309300971526937, 3.303125000614517415 ) ) ;
#9024 = EDGE_CURVE ( 'NONE', #6329, #3747, #8211, .T. ) ;
#9025 = ORIENTED_EDGE ( 'NONE', *, *, #3108, .F. ) ;
#9026 = CARTESIAN_POINT ( 'NONE',  ( 46.99999999999995737, 90.00000000000000000, -8.000000000000000000 ) ) ;
#9027 = ORIENTED_EDGE ( 'NONE', *, *, #9374, .T. ) ;
#9028 = CARTESIAN_POINT ( 'NONE',  ( -998.3826497308103853, 0.000000000000000000, 0.000000000000000000 ) ) ;
#9029 = CARTESIAN_POINT ( 'NONE',  ( 66.44356964375000985, 71.84604660189820891, 3.190625000614517592 ) ) ;
#9030 = CIRCLE ( 'NONE', #2986, 3.350000000000003642 ) ;
#9031 = CARTESIAN_POINT ( 'NONE',  ( 3.800000000000015365, 90.00000000000000000, 3.762500001229034385 ) ) ;
#9032 = EDGE_CURVE ( 'NONE', #5860, #11494, #6242, .T. ) ;
#9033 = CARTESIAN_POINT ( 'NONE',  ( 2.168404344971008868E-16, 0.000000000000000000, 0.000000000000000000 ) ) ;
#9034 = EDGE_LOOP ( 'NONE', ( #11231, #11174, #9458, #5291 ) ) ;
#9035 = CARTESIAN_POINT ( 'NONE',  ( 66.20000000000000284, 71.98667160128370313, 4.287500000000000533 ) ) ;
#9036 = DIRECTION ( 'NONE',  ( -0.000000000000000000, 1.000000000000000000, -0.000000000000000000 ) ) ;
#9037 = DIRECTION ( 'NONE',  ( -0.000000000000000000, -0.000000000000000000, -1.000000000000000000 ) ) ;
#9038 = ORIENTED_EDGE ( 'NONE', *, *, #6590, .T. ) ;
#9039 = ADVANCED_FACE ( 'NONE', ( #3570 ), #11075, .F. ) ;
#9040 = STYLED_ITEM ( 'NONE', ( #10573 ), #7935 ) ;
#9041 = LINE ( 'NONE', #4277, #2583 ) ;
#9042 = ORIENTED_EDGE ( 'NONE', *, *, #12906, .F. ) ;
#9043 = CARTESIAN_POINT ( 'NONE',  ( 0.1698013801012111523, -5.473461295629626022, -0.8000000000000000444 ) ) ;
#9044 = CARTESIAN_POINT ( 'NONE',  ( 66.44356964374999563, 90.00000000000000000, 3.678125000614516971 ) ) ;
#9045 = VERTEX_POINT ( 'NONE', #12525 ) ;
#9046 = CARTESIAN_POINT ( 'NONE',  ( 3.556430356250014579, 108.1539533981018053, 4.371875000614517504 ) ) ;
#9047 = DIRECTION ( 'NONE',  ( -0.000000000000000000, -0.000000000000000000, -1.000000000000000000 ) ) ;
#9048 = DIRECTION ( 'NONE',  ( 0.000000000000000000, 0.000000000000000000, 1.000000000000000000 ) ) ;
#9049 = CARTESIAN_POINT ( 'NONE',  ( 35.00000000000000000, 90.00000000000000000, 5.000000000000000000 ) ) ;
#9050 = AXIS2_PLACEMENT_3D ( 'NONE', #5250, #7280, #10084 ) ;
#9051 = CARTESIAN_POINT ( 'NONE',  ( 17.66025403784438197, 77.14656965084323303, 1.000000000000000000 ) ) ;
#9052 = EDGE_CURVE ( 'NONE', #7127, #8087, #536, .T. ) ;
#9053 = CARTESIAN_POINT ( 'NONE',  ( -32.99038105676694954, 57.14101615137754209, -1.000000000000000000 ) ) ;
#9054 = AXIS2_PLACEMENT_3D ( 'NONE', #7489, #10432, #7358 ) ;
#9055 = DIRECTION ( 'NONE',  ( 0.000000000000000000, -1.000000000000000000, 0.000000000000000000 ) ) ;
#9056 = DIRECTION ( 'NONE',  ( 0.5877852522924770229, 0.8090169943749445647, 0.000000000000000000 ) ) ;
#9057 = EDGE_CURVE ( 'NONE', #4963, #12297, #1661, .T. ) ;
#9058 = ORIENTED_EDGE ( 'NONE', *, *, #4742, .T. ) ;
#9059 = FACE_OUTER_BOUND ( 'NONE', #2312, .T. ) ;
#9060 = ORIENTED_EDGE ( 'NONE', *, *, #10942, .F. ) ;
#9061 = CIRCLE ( 'NONE', #10736, 1.599999999999990319 ) ;
#9062 = PRESENTATION_STYLE_ASSIGNMENT (( #11153 ) ) ;
#9063 = COLOUR_RGB ( '',0.8941176470588234615, 0.8941176470588234615, 0.8941176470588234615 ) ;
#9064 = EDGE_CURVE ( 'NONE', #10795, #10977, #1940, .T. ) ;
#9065 = CARTESIAN_POINT ( 'NONE',  ( 0.000000000000000000, -0.5773502691896256200, -1.000000000000000000 ) ) ;
#9066 = DIRECTION ( 'NONE',  ( -0.000000000000000000, 1.000000000000000000, -0.000000000000000000 ) ) ;
#9067 = LINE ( 'NONE', #11225, #9477 ) ;
#9068 = ORIENTED_EDGE ( 'NONE', *, *, #12870, .F. ) ;
#9069 = AXIS2_PLACEMENT_3D ( 'NONE', #3518, #8613, #7501 ) ;
#9070 = DIRECTION ( 'NONE',  ( 0.000000000000000000, -1.000000000000000000, -0.000000000000000000 ) ) ;
#9071 = CARTESIAN_POINT ( 'NONE',  ( 50.59999999999999432, 117.0199925980744666, 4.062500001229034652 ) ) ;
#9072 = EDGE_CURVE ( 'NONE', #7376, #2423, #9701, .T. ) ;
#9073 = VERTEX_POINT ( 'NONE', #6496 ) ;
#9074 = FACE_OUTER_BOUND ( 'NONE', #12679, .T. ) ;
#9075 = EDGE_CURVE ( 'NONE', #11004, #8177, #12657, .T. ) ;
#9076 = ORIENTED_EDGE ( 'NONE', *, *, #9147, .F. ) ;
#9077 = ORIENTED_EDGE ( 'NONE', *, *, #2858, .F. ) ;
#9078 = CARTESIAN_POINT ( 'NONE',  ( 0.000000000000000000, 0.000000000000000000, 0.000000000000000000 ) ) ;
#9079 = CARTESIAN_POINT ( 'NONE',  ( 67.70000000000001705, 90.00000000000000000, 8.000000000000000000 ) ) ;
#9080 = VECTOR ( 'NONE', #6723, 1000.000000000000000 ) ;
#9081 = EDGE_LOOP ( 'NONE', ( #9025, #930, #4339, #2705 ) ) ;
#9082 = AXIS2_PLACEMENT_3D ( 'NONE', #5760, #10856, #12822 ) ;
#9083 = ORIENTED_EDGE ( 'NONE', *, *, #8286, .F. ) ;
#9084 = CARTESIAN_POINT ( 'NONE',  ( -63.73205080756886076, 30.46410161513775350, 0.000000000000000000 ) ) ;
#9085 = ORIENTED_EDGE ( 'NONE', *, *, #7874, .F. ) ;
#9086 = APPLICATION_PROTOCOL_DEFINITION ( 'draft international standard', 'automotive_design', 1998, #7514 ) ;
#9087 = CARTESIAN_POINT ( 'NONE',  ( 66.44356964374999563, 90.00000000000000000, 4.578125000614516438 ) ) ;
#9088 = EDGE_CURVE ( 'NONE', #3524, #7014, #10685, .T. ) ;
#9089 = ORIENTED_EDGE ( 'NONE', *, *, #1153, .T. ) ;
#9090 = CIRCLE ( 'NONE', #10134, 0.1000000000000000472 ) ;
#9091 = CARTESIAN_POINT ( 'NONE',  ( 3.000000000000004441, 2.000000000000000000, -8.000000000000000000 ) ) ;
#9092 = ORIENTED_EDGE ( 'NONE', *, *, #5975, .F. ) ;
#9093 = CIRCLE ( 'NONE', #1141, 3.349999999999995204 ) ;
#9094 = EDGE_CURVE ( 'NONE', #4025, #12399, #22, .T. ) ;
#9095 = CARTESIAN_POINT ( 'NONE',  ( 7.650000000000000355, 0.000000000000000000, 1.219500000000000028 ) ) ;
#9096 = CARTESIAN_POINT ( 'NONE',  ( -1.000000000000000000, -4.873461295629625489, -0.8000000000000000444 ) ) ;
#9097 = CARTESIAN_POINT ( 'NONE',  ( 48.49999999999995737, 90.00000000000000000, -8.000000000000000000 ) ) ;
#9098 = CARTESIAN_POINT ( 'NONE',  ( 45.00000000000000000, -5.000000000000000000, 5.750000000000000888 ) ) ;
#9099 = VECTOR ( 'NONE', #5587, 1000.000000000000000 ) ;
#9100 = DIRECTION ( 'NONE',  ( 1.000000000000000000, 0.000000000000000000, -0.000000000000000000 ) ) ;
#9101 = EDGE_LOOP ( 'NONE', ( #12050, #6352, #12313, #1936, #151, #7716, #650, #11784 ) ) ;
#9102 = AXIS2_PLACEMENT_3D ( 'NONE', #8291, #1282, #6316 ) ;
#9103 = CARTESIAN_POINT ( 'NONE',  ( 19.27821517812500574, 117.2309300971526937, 4.334375000614516971 ) ) ;
#9104 = CARTESIAN_POINT ( 'NONE',  ( 50.59999999999999432, 117.0199925980744666, 3.050000000000000266 ) ) ;
#9105 = FACE_OUTER_BOUND ( 'NONE', #7623, .T. ) ;
#9106 = ORIENTED_EDGE ( 'NONE', *, *, #9963, .F. ) ;
#9107 = DIRECTION ( 'NONE',  ( 0.000000000000000000, 0.000000000000000000, 1.000000000000000000 ) ) ;
#9108 = VERTEX_POINT ( 'NONE', #11605 ) ;
#9109 = CARTESIAN_POINT ( 'NONE',  ( -60.00000000000000000, -6.000000000000000000, -15.00000000000000355 ) ) ;
#9110 = CARTESIAN_POINT ( 'NONE',  ( 19.27821517812500574, 117.2309300971526937, 3.378125000614517148 ) ) ;
#9111 = ORIENTED_EDGE ( 'NONE', *, *, #5699, .F. ) ;
#9112 = VECTOR ( 'NONE', #12411, 1000.000000000000000 ) ;
#9113 = CARTESIAN_POINT ( 'NONE',  ( 3.556430356250028790, 71.84604660189818048, 3.546875000614516882 ) ) ;
#9114 = CARTESIAN_POINT ( 'NONE',  ( -48.33333333333332860, 2.000000000000000000, -1.734723475976807094E-15 ) ) ;
#9115 = EDGE_CURVE ( 'NONE', #655, #11127, #2581, .T. ) ;
#9116 = CARTESIAN_POINT ( 'NONE',  ( 5.000000000000007994, 90.00000000000000000, 4.000000000000000000 ) ) ;
#9117 = ADVANCED_FACE ( 'NONE', ( #10428 ), #9512, .F. ) ;
#9118 = DIRECTION ( 'NONE',  ( 0.000000000000000000, -0.000000000000000000, -1.000000000000000000 ) ) ;
#9119 = DIRECTION ( 'NONE',  ( 0.000000000000000000, 0.000000000000000000, 1.000000000000000000 ) ) ;
#9120 = CARTESIAN_POINT ( 'NONE',  ( -60.00000000000000000, 23.99999999999998934, 2.500000000000000000 ) ) ;
#9121 = AXIS2_PLACEMENT_3D ( 'NONE', #12927, #6967, #11818 ) ;
#9122 = LINE ( 'NONE', #7293, #2634 ) ;
#9123 = FACE_OUTER_BOUND ( 'NONE', #4439, .T. ) ;
#9124 = CARTESIAN_POINT ( 'NONE',  ( -28.99038105676692112, 50.21281292110204930, 1.000000000000000000 ) ) ;
#9125 = VERTEX_POINT ( 'NONE', #10490 ) ;
#9126 = DIRECTION ( 'NONE',  ( -1.000000000000000000, 0.000000000000000000, 0.000000000000000000 ) ) ;
#9127 = EDGE_LOOP ( 'NONE', ( #5467, #4810, #1835, #12054 ) ) ;
#9128 = CIRCLE ( 'NONE', #3506, 1.500000000000001332 ) ;
#9129 = LINE ( 'NONE', #6252, #3111 ) ;
#9130 = CARTESIAN_POINT ( 'NONE',  ( 45.00000000000000000, 0.000000000000000000, 5.750000000000000888 ) ) ;
#9131 = EDGE_CURVE ( 'NONE', #1106, #488, #6453, .T. ) ;
#9132 = LINE ( 'NONE', #8356, #5919 ) ;
#9133 = ORIENTED_EDGE ( 'NONE', *, *, #12555, .T. ) ;
#9134 = DIRECTION ( 'NONE',  ( 0.000000000000000000, 0.000000000000000000, 1.000000000000000000 ) ) ;
#9135 = CARTESIAN_POINT ( 'NONE',  ( -6.666666666666660745, 0.000000000000000000, 0.000000000000000000 ) ) ;
#9136 = AXIS2_PLACEMENT_3D ( 'NONE', #6311, #9326, #8217 ) ;
#9137 = VERTEX_POINT ( 'NONE', #667 ) ;
#9138 =( LENGTH_UNIT ( ) NAMED_UNIT ( * ) SI_UNIT ( .MILLI., .METRE. ) );
#9139 = ORIENTED_EDGE ( 'NONE', *, *, #5797, .T. ) ;
#9140 = DIRECTION ( 'NONE',  ( -0.000000000000000000, -1.000000000000000000, -0.000000000000000000 ) ) ;
#9141 = ORIENTED_EDGE ( 'NONE', *, *, #3130, .F. ) ;
#9142 = CARTESIAN_POINT ( 'NONE',  ( 30.78620769635677235, 85.05086326499690585, -1.000000000000000000 ) ) ;
#9143 = DIRECTION ( 'NONE',  ( -0.000000000000000000, -1.000000000000000000, -0.000000000000000000 ) ) ;
#9144 = ADVANCED_FACE ( 'NONE', ( #3699 ), #4476, .T. ) ;
#9145 = VERTEX_POINT ( 'NONE', #9640 ) ;
#9146 = VECTOR ( 'NONE', #12383, 1000.000000000000000 ) ;
#9147 = EDGE_CURVE ( 'NONE', #9996, #10107, #3124, .T. ) ;
#9148 = ORIENTED_EDGE ( 'NONE', *, *, #7681, .T. ) ;
#9149 = CARTESIAN_POINT ( 'NONE',  ( 3.350000000000000089, 0.000000000000000000, -0.8000000000000000444 ) ) ;
#9150 = ORIENTED_EDGE ( 'NONE', *, *, #12108, .T. ) ;
#9151 = SHAPE_DEFINITION_REPRESENTATION ( #12421, #5582 ) ;
#9152 = CARTESIAN_POINT ( 'NONE',  ( 66.44356964374999563, 90.00000000000000000, 4.128125000614517148 ) ) ;
#9153 = ORIENTED_EDGE ( 'NONE', *, *, #11152, .F. ) ;
#9154 = CARTESIAN_POINT ( 'NONE',  ( 35.00000000000000000, 90.00000000000000000, 4.000000000000000000 ) ) ;
#9155 = CARTESIAN_POINT ( 'NONE',  ( -0.1038759689922479496, -3.348389132562988646, 0.000000000000000000 ) ) ;
#9156 = VERTEX_POINT ( 'NONE', #12459 ) ;
#9157 = DIRECTION ( 'NONE',  ( -0.000000000000000000, -0.000000000000000000, -1.000000000000000000 ) ) ;
#9158 = CARTESIAN_POINT ( 'NONE',  ( 35.00000000000000000, 126.3079067962036106, 4.690625000614517148 ) ) ;
#9159 = CARTESIAN_POINT ( 'NONE',  ( 31.86869970978804290, 88.80942934165229019, 4.800000000000000711 ) ) ;
#9160 = PLANE ( 'NONE',  #12909 ) ;
#9161 =( NAMED_UNIT ( * ) SI_UNIT ( $, .STERADIAN. ) SOLID_ANGLE_UNIT ( ) );
#9162 = EDGE_CURVE ( 'NONE', #11802, #12915, #9577, .T. ) ;
#9163 = DIRECTION ( 'NONE',  ( -0.8660254037844365982, -0.5000000000000036637, 0.000000000000000000 ) ) ;
#9164 = AXIS2_PLACEMENT_3D ( 'NONE', #3352, #6405, #5166 ) ;
#9165 = VERTEX_POINT ( 'NONE', #1526 ) ;
#9166 = CARTESIAN_POINT ( 'NONE',  ( 35.00000000000000711, 53.97334320256736362, 3.312500000000000000 ) ) ;
#9167 = VERTEX_POINT ( 'NONE', #11470 ) ;
#9168 = FACE_OUTER_BOUND ( 'NONE', #10137, .T. ) ;
#9169 = ORIENTED_EDGE ( 'NONE', *, *, #12451, .T. ) ;
#9170 = DIRECTION ( 'NONE',  ( -0.000000000000000000, -0.000000000000000000, -1.000000000000000000 ) ) ;
#9171 = ORIENTED_EDGE ( 'NONE', *, *, #3260, .T. ) ;
#9172 = VECTOR ( 'NONE', #5127, 1000.000000000000000 ) ;
#9173 = DIRECTION ( 'NONE',  ( -0.000000000000000000, -1.000000000000000000, -0.000000000000000000 ) ) ;
#9174 = UNCERTAINTY_MEASURE_WITH_UNIT (LENGTH_MEASURE( 1.000000000000000082E-05 ), #9424, 'distance_accuracy_value', 'NONE');
#9175 = CARTESIAN_POINT ( 'NONE',  ( 19.27821517812500574, 117.2309300971526937, 3.828125000614516882 ) ) ;
#9176 = VERTEX_POINT ( 'NONE', #2715 ) ;
#9177 = AXIS2_PLACEMENT_3D ( 'NONE', #12115, #1311, #5547 ) ;
#9178 = CARTESIAN_POINT ( 'NONE',  ( 3.556430356250014579, 108.1539533981018053, 4.821875000614516793 ) ) ;
#9179 = PLANE ( 'NONE',  #10406 ) ;
#9180 = EDGE_CURVE ( 'NONE', #12248, #1413, #6690, .T. ) ;
#9181 = LINE ( 'NONE', #2194, #2067 ) ;
#9182 = AXIS2_PLACEMENT_3D ( 'NONE', #2115, #7143, #11125 ) ;
#9183 = DIRECTION ( 'NONE',  ( -0.8090169943749485615, 0.5877852522924716938, 0.000000000000000000 ) ) ;
#9184 = CYLINDRICAL_SURFACE ( 'NONE', #1867, 31.19999999999999929 ) ;
#9185 = CARTESIAN_POINT ( 'NONE',  ( 31.65768047819777919, 88.96129878493390208, 4.800000000000000711 ) ) ;
#9186 = DIRECTION ( 'NONE',  ( 0.03100775193798452692, 0.9995191440486532741, 0.000000000000000000 ) ) ;
#9187 = ADVANCED_FACE ( 'NONE', ( #3438 ), #2521, .F. ) ;
#9188 = EDGE_CURVE ( 'NONE', #11115, #7727, #10747, .T. ) ;
#9189 = CARTESIAN_POINT ( 'NONE',  ( 52.45028081366923089, 66.83239978927284142, 2.333333333333333481 ) ) ;
#9190 = FACE_OUTER_BOUND ( 'NONE', #9233, .T. ) ;
#9191 = VERTEX_POINT ( 'NONE', #3953 ) ;
#9192 = CIRCLE ( 'NONE', #2095, 1.599999999999997202 ) ;
#9193 = CARTESIAN_POINT ( 'NONE',  ( 0.1038759689922479496, -3.348389132562988646, -0.8000000000000000444 ) ) ;
#9194 = EDGE_LOOP ( 'NONE', ( #4296, #9092, #7525, #7779 ) ) ;
#9195 = SURFACE_SIDE_STYLE ('',( #3123 ) ) ;
#9196 = EDGE_CURVE ( 'NONE', #7336, #8306, #8137, .T. ) ;
#9197 = CARTESIAN_POINT ( 'NONE',  ( 31.86869970978804290, 88.80942934165229019, 4.800000000000000711 ) ) ;
#9198 = CARTESIAN_POINT ( 'NONE',  ( 35.00000000000000000, 126.0266567974326222, 4.100000001229034297 ) ) ;
#9199 = DIRECTION ( 'NONE',  ( 0.000000000000000000, 0.000000000000000000, -1.000000000000000000 ) ) ;
#9200 = VECTOR ( 'NONE', #11016, 1000.000000000000000 ) ;
#9201 = EDGE_LOOP ( 'NONE', ( #8231, #3086, #7444, #6600 ) ) ;
#9202 = DIRECTION ( 'NONE',  ( -0.3262398754384820410, 0.9452870165584015272, 0.000000000000000000 ) ) ;
#9203 = CARTESIAN_POINT ( 'NONE',  ( -3.666666666666658969, 64.83346624110779999, 1.000000000000000000 ) ) ;
#9204 = VERTEX_POINT ( 'NONE', #7742 ) ;
#9205 = DIRECTION ( 'NONE',  ( 0.4719909656437444867, -0.8816033849473842166, 0.000000000000000000 ) ) ;
#9206 = VERTEX_POINT ( 'NONE', #2596 ) ;
#9207 = EDGE_LOOP ( 'NONE', ( #12022, #12630, #11625, #323 ) ) ;
#9208 = EDGE_CURVE ( 'NONE', #3791, #2398, #2736, .T. ) ;
#9209 = CARTESIAN_POINT ( 'NONE',  ( 1.040000000000000036, -0.5773502691896255090, 1.000000000000000000 ) ) ;
#9210 = VECTOR ( 'NONE', #3426, 1000.000000000000000 ) ;
#9211 = DIRECTION ( 'NONE',  ( 1.000000000000000000, 0.000000000000000000, 0.000000000000000000 ) ) ;
#9212 = EDGE_LOOP ( 'NONE', ( #1771, #4260, #5934, #7326 ) ) ;
#9213 = ORIENTED_EDGE ( 'NONE', *, *, #3328, .T. ) ;
#9214 = CARTESIAN_POINT ( 'NONE',  ( 65.00000000000000000, 90.00000000000000000, 4.000000000000000000 ) ) ;
#9215 = EDGE_LOOP ( 'NONE', ( #11259, #7747, #7805, #6956, #12419, #6472, #8090, #8493, #2226, #6321, #2057, #4657 ) ) ;
#9216 =( NAMED_UNIT ( * ) SI_UNIT ( $, .STERADIAN. ) SOLID_ANGLE_UNIT ( ) );
#9217 = CARTESIAN_POINT ( 'NONE',  ( 66.44356964374998142, 108.1539533981018053, 3.715625000614517948 ) ) ;
#9218 = ORIENTED_EDGE ( 'NONE', *, *, #9788, .T. ) ;
#9219 = AXIS2_PLACEMENT_3D ( 'NONE', #9028, #5888, #9881 ) ;
#9220 = ADVANCED_FACE ( 'NONE', ( #10022 ), #4987, .F. ) ;
#9221 = FACE_OUTER_BOUND ( 'NONE', #11438, .T. ) ;
#9222 = LINE ( 'NONE', #5297, #9794 ) ;
#9223 = ORIENTED_EDGE ( 'NONE', *, *, #2943, .T. ) ;
#9224 = CARTESIAN_POINT ( 'NONE',  ( 0.000000000000000000, 0.000000000000000000, 0.000000000000000000 ) ) ;
#9225 = CARTESIAN_POINT ( 'NONE',  ( 35.00000000000000711, 53.69209320379639649, 4.465625000614517504 ) ) ;
#9226 = EDGE_CURVE ( 'NONE', #12533, #5692, #8847, .T. ) ;
#9227 = CARTESIAN_POINT ( 'NONE',  ( 3.000000000000004441, 30.00000000000000000, 2.500000000000000000 ) ) ;
#9228 = PLANE ( 'NONE',  #581 ) ;
#9229 = PRESENTATION_LAYER_ASSIGNMENT (  '', '', ( #6706 ) ) ;
#9230 = PLANE ( 'NONE',  #4997 ) ;
#9231 = EDGE_LOOP ( 'NONE', ( #11897, #6135 ) ) ;
#9232 = CARTESIAN_POINT ( 'NONE',  ( 66.44356964374999563, 90.00000000000000000, 4.634375000614516793 ) ) ;
#9233 = EDGE_LOOP ( 'NONE', ( #8729, #510, #5566, #9898, #10413, #4626 ) ) ;
#9234 = DIRECTION ( 'NONE',  ( -0.000000000000000000, 0.000000000000000000, -1.000000000000000000 ) ) ;
#9235 = ORIENTED_EDGE ( 'NONE', *, *, #4232, .T. ) ;
#9236 = CARTESIAN_POINT ( 'NONE',  ( 45.00000000000000000, 2.000000000000000000, -5.750000000000000000 ) ) ;
#9237 = ORIENTED_EDGE ( 'NONE', *, *, #4635, .T. ) ;
#9238 = EDGE_CURVE ( 'NONE', #4244, #7837, #2968, .T. ) ;
#9239 = CIRCLE ( 'NONE', #11319, 0.1000000000000000472 ) ;
#9240 = CARTESIAN_POINT ( 'NONE',  ( 0.000000000000000000, 0.000000000000000000, 10.00000000000000000 ) ) ;
#9241 = CARTESIAN_POINT ( 'NONE',  ( 3.556430356250014579, 108.1539533981018053, 2.965625000614517504 ) ) ;
#9242 = EDGE_CURVE ( 'NONE', #330, #8478, #1053, .T. ) ;
#9243 = CARTESIAN_POINT ( 'NONE',  ( 3.556430356250014579, 108.1539533981018053, 3.921875000614517326 ) ) ;
#9244 = DIRECTION ( 'NONE',  ( 1.000000000000000000, 0.000000000000000000, 0.000000000000000000 ) ) ;
#9245 = CARTESIAN_POINT ( 'NONE',  ( -16.33333333333332504, 30.00000000000000000, 7.999999999999996447 ) ) ;
#9246 = AXIS2_PLACEMENT_3D ( 'NONE', #9487, #1574, #9747 ) ;
#9247 =( BOUNDED_CURVE ( )  B_SPLINE_CURVE ( 2, ( #7013, #7139, #124, #11057, #3227, #4075, #10993 ),
 .UNSPECIFIED., .F., .F. ) 
 B_SPLINE_CURVE_WITH_KNOTS ( ( 3, 2, 2, 3 ),
 ( 0.3000000000000002109, 0.3333333333333334259, 0.3666666666666666963, 0.3999999999999999667 ),
 .UNSPECIFIED. ) 
 CURVE ( )  GEOMETRIC_REPRESENTATION_ITEM ( )  RATIONAL_B_SPLINE_CURVE ( ( 0.9999999999999991118, 0.8660254037844395958, 1.000000000000000000, 0.8660254037844387076, 1.000000000000000000, 0.8660254037844389297, 0.9999999999999997780 ) ) 
 REPRESENTATION_ITEM ( '' )  );
#9248 = CARTESIAN_POINT ( 'NONE',  ( -9.666666666666657193, 79.07477288111861924, -1.000000000000000000 ) ) ;
#9249 = LINE ( 'NONE', #8148, #6689 ) ;
#9250 = LINE ( 'NONE', #273, #11582 ) ;
#9251 = DIRECTION ( 'NONE',  ( 0.000000000000000000, 0.000000000000000000, -1.000000000000000000 ) ) ;
#9252 = ADVANCED_FACE ( 'NONE', ( #989 ), #8000, .F. ) ;
#9253 = DIRECTION ( 'NONE',  ( 0.000000000000000000, 0.000000000000000000, 1.000000000000000000 ) ) ;
#9254 = FACE_OUTER_BOUND ( 'NONE', #8297, .T. ) ;
#9255 = EDGE_LOOP ( 'NONE', ( #9587, #11698, #10105, #8962 ) ) ;
#9256 = VECTOR ( 'NONE', #3978, 1000.000000000000000 ) ;
#9257 = EDGE_CURVE ( 'NONE', #7589, #7916, #7016, .T. ) ;
#9258 = CARTESIAN_POINT ( 'NONE',  ( -60.00000000000000000, 30.00000000000000000, -8.000000000000003553 ) ) ;
#9259 = ORIENTED_EDGE ( 'NONE', *, *, #214, .F. ) ;
#9260 =( LENGTH_UNIT ( ) NAMED_UNIT ( * ) SI_UNIT ( .MILLI., .METRE. ) );
#9261 = AXIS2_PLACEMENT_3D ( 'NONE', #12745, #764, #6911 ) ;
#9262 = EDGE_CURVE ( 'NONE', #443, #12930, #5046, .T. ) ;
#9263 = DIRECTION ( 'NONE',  ( 0.5000000000000038858, -0.8660254037844362651, 0.000000000000000000 ) ) ;
#9264 = DIRECTION ( 'NONE',  ( 0.000000000000000000, 0.000000000000000000, 1.000000000000000000 ) ) ;
#9265 = CARTESIAN_POINT ( 'NONE',  ( 1.269999999999999796, 2.849999999999999645, 0.000000000000000000 ) ) ;
#9266 = COLOUR_RGB ( '',0.8941176470588234615, 0.8941176470588234615, 0.8941176470588234615 ) ;
#9267 = ORIENTED_EDGE ( 'NONE', *, *, #5434, .F. ) ;
#9268 = CARTESIAN_POINT ( 'NONE',  ( -32.99038105676694954, 57.14101615137754209, 1.000000000000000000 ) ) ;
#9269 = CARTESIAN_POINT ( 'NONE',  ( 35.00000000000000000, 90.00000000000000000, 8.000000000000000000 ) ) ;
#9270 = ORIENTED_EDGE ( 'NONE', *, *, #3830, .T. ) ;
#9271 = CARTESIAN_POINT ( 'NONE',  ( 0.000000000000000000, 0.000000000000000000, 0.000000000000000000 ) ) ;
#9272 = AXIS2_PLACEMENT_3D ( 'NONE', #8161, #7243, #2142 ) ;
#9273 = DIRECTION ( 'NONE',  ( 1.000000000000000000, -0.000000000000000000, -0.000000000000000000 ) ) ;
#9274 = ORIENTED_EDGE ( 'NONE', *, *, #4723, .F. ) ;
#9275 = ORIENTED_EDGE ( 'NONE', *, *, #9374, .F. ) ;
#9276 = SPHERICAL_SURFACE ( 'NONE', #11963, 3.351416843938787249 ) ;
#9277 = ORIENTED_EDGE ( 'NONE', *, *, #2803, .T. ) ;
#9278 = DIRECTION ( 'NONE',  ( -2.891205793294678696E-17, 0.000000000000000000, 1.000000000000000000 ) ) ;
#9279 = ORIENTED_EDGE ( 'NONE', *, *, #1473, .T. ) ;
#9280 = EDGE_CURVE ( 'NONE', #6649, #309, #9600, .T. ) ;
#9281 = EDGE_CURVE ( 'NONE', #370, #12297, #1235, .T. ) ;
#9282 = AXIS2_PLACEMENT_3D ( 'NONE', #8736, #7952, #9781 ) ;
#9283 = PRODUCT_DEFINITION_SHAPE ( 'NONE', 'NONE',  #10255 ) ;
#9284 = ORIENTED_EDGE ( 'NONE', *, *, #11078, .T. ) ;
#9285 = CONICAL_SURFACE ( 'NONE', #3860, 1.500000000000001332, 1.029744260000000633 ) ;
#9286 = CARTESIAN_POINT ( 'NONE',  ( -6.666666666666660745, 0.000000000000000000, 1.499999999999999556 ) ) ;
#9287 = VERTEX_POINT ( 'NONE', #3759 ) ;
#9288 = CARTESIAN_POINT ( 'NONE',  ( 3.800000000000015365, 108.0133283987163111, 4.625000001229034652 ) ) ;
#9289 = EDGE_LOOP ( 'NONE', ( #6167, #12228, #6985, #9989 ) ) ;
#9290 = DIRECTION ( 'NONE',  ( -0.000000000000000000, 1.000000000000000000, -0.000000000000000000 ) ) ;
#9291 = ORIENTED_EDGE ( 'NONE', *, *, #2481, .F. ) ;
#9292 = PLANE ( 'NONE',  #2962 ) ;
#9293 = VECTOR ( 'NONE', #9611, 1000.000000000000000 ) ;
#9294 = AXIS2_PLACEMENT_3D ( 'NONE', #5823, #9751, #8708 ) ;
#9295 = CARTESIAN_POINT ( 'NONE',  ( 19.40000000000000924, 117.0199925980744666, 3.237500001229034030 ) ) ;
#9296 = CARTESIAN_POINT ( 'NONE',  ( 40.00000000000000000, 90.00000000000000000, -8.000000000000000000 ) ) ;
#9297 = CYLINDRICAL_SURFACE ( 'NONE', #7899, 31.19999999999999929 ) ;
#9298 = VERTEX_POINT ( 'NONE', #2048 ) ;
#9299 = CARTESIAN_POINT ( 'NONE',  ( 66.19999999999998863, 90.00000000000000000, 3.425000000000000266 ) ) ;
#9300 = ORIENTED_EDGE ( 'NONE', *, *, #9802, .F. ) ;
#9301 = VECTOR ( 'NONE', #8359, 1000.000000000000000 ) ;
#9302 = EDGE_CURVE ( 'NONE', #1989, #9204, #922, .T. ) ;
#9303 = DIRECTION ( 'NONE',  ( -1.000000000000000000, -0.000000000000000000, -0.000000000000000000 ) ) ;
#9304 = EDGE_LOOP ( 'NONE', ( #10315, #7809, #6224 ) ) ;
#9305 = AXIS2_PLACEMENT_3D ( 'NONE', #11903, #717, #2761 ) ;
#9306 = DIRECTION ( 'NONE',  ( 1.000000000000000000, 0.000000000000000000, 5.337610695313252124E-17 ) ) ;
#9307 = ORIENTED_EDGE ( 'NONE', *, *, #4122, .F. ) ;
#9308 = CARTESIAN_POINT ( 'NONE',  ( 34.25000000000000000, 92.49999999999998579, 4.000000000000000000 ) ) ;
#9309 = PLANE ( 'NONE',  #2022 ) ;
#9310 = LINE ( 'NONE', #7348, #9661 ) ;
#9311 = DIRECTION ( 'NONE',  ( 0.000000000000000000, 0.000000000000000000, 1.000000000000000000 ) ) ;
#9312 = AXIS2_PLACEMENT_3D ( 'NONE', #10950, #11876, #875 ) ;
#9313 = CARTESIAN_POINT ( 'NONE',  ( 44.16515138991168499, 94.00000000000000000, -10.00000000000000000 ) ) ;
#9314 = COLOUR_RGB ( '',0.8941176470588234615, 0.8941176470588234615, 0.8941176470588234615 ) ;
#9315 = ADVANCED_FACE ( 'NONE', ( #1791, #11858 ), #12780, .T. ) ;
#9316 = EDGE_CURVE ( 'NONE', #4104, #1224, #5185, .T. ) ;
#9317 = LINE ( 'NONE', #2387, #1976 ) ;
#9318 = EDGE_CURVE ( 'NONE', #2314, #8971, #10873, .T. ) ;
#9319 = CARTESIAN_POINT ( 'NONE',  ( 35.00000000000000000, 90.00000000000000000, 4.800000000000000711 ) ) ;
#9320 = LINE ( 'NONE', #11279, #4276 ) ;
#9321 = LINE ( 'NONE', #274, #521 ) ;
#9322 = CIRCLE ( 'NONE', #6812, 1.599999999999990319 ) ;
#9323 = CARTESIAN_POINT ( 'NONE',  ( 36.50000000000001421, 79.80000000000001137, 8.000000000000000000 ) ) ;
#9324 = CARTESIAN_POINT ( 'NONE',  ( 64.24207199149496716, 100.8784753363798075, 2.999999999999999556 ) ) ;
#9325 = EDGE_LOOP ( 'NONE', ( #1076, #11369, #3809, #132, #12105 ) ) ;
#9326 = DIRECTION ( 'NONE',  ( 1.000000000000000000, 0.000000000000000000, -0.000000000000000000 ) ) ;
#9327 = VERTEX_POINT ( 'NONE', #9890 ) ;
#9328 =( NAMED_UNIT ( * ) PLANE_ANGLE_UNIT ( ) SI_UNIT ( $, .RADIAN. ) );
#9329 = EDGE_CURVE ( 'NONE', #4968, #3844, #8339, .T. ) ;
#9330 = FACE_OUTER_BOUND ( 'NONE', #6630, .T. ) ;
#9331 = DIRECTION ( 'NONE',  ( -0.000000000000000000, 1.000000000000000000, -0.000000000000000000 ) ) ;
#9332 = DIRECTION ( 'NONE',  ( 0.000000000000000000, -1.000000000000000000, 0.000000000000000000 ) ) ;
#9333 = ORIENTED_EDGE ( 'NONE', *, *, #5118, .F. ) ;
#9334 = CARTESIAN_POINT ( 'NONE',  ( 35.00000000000000000, 90.00000000000000000, -1.000000000000000000 ) ) ;
#9335 = DIRECTION ( 'NONE',  ( 0.000000000000000000, 0.000000000000000000, 1.000000000000000000 ) ) ;
#9336 = ORIENTED_EDGE ( 'NONE', *, *, #2250, .T. ) ;
#9337 = DIRECTION ( 'NONE',  ( 1.000000000000000000, 0.000000000000000000, 0.000000000000000000 ) ) ;
#9338 = DIRECTION ( 'NONE',  ( 0.4999999999999995559, -0.8660254037844389297, 0.000000000000000000 ) ) ;
#9339 = VERTEX_POINT ( 'NONE', #6157 ) ;
#9340 = VECTOR ( 'NONE', #7826, 1000.000000000000000 ) ;
#9341 = ORIENTED_EDGE ( 'NONE', *, *, #11905, .T. ) ;
#9342 = CARTESIAN_POINT ( 'NONE',  ( 3.800000000000015365, 90.00000000000000000, 2.862500001229034474 ) ) ;
#9343 = DIRECTION ( 'NONE',  ( -1.000000000000000000, 0.000000000000000000, 0.000000000000000000 ) ) ;
#9344 = VERTEX_POINT ( 'NONE', #1383 ) ;
#9345 = EDGE_CURVE ( 'NONE', #3991, #9740, #4589, .T. ) ;
#9346 = ORIENTED_EDGE ( 'NONE', *, *, #464, .T. ) ;
#9347 = AXIS2_PLACEMENT_3D ( 'NONE', #8089, #7166, #1142 ) ;
#9348 = DIRECTION ( 'NONE',  ( -1.000000000000000000, 0.000000000000000000, 0.000000000000000000 ) ) ;
#9349 = EDGE_LOOP ( 'NONE', ( #11919, #10978, #10934 ) ) ;
#9350 = CARTESIAN_POINT ( 'NONE',  ( 37.73448666702899601, 121.2272378967086013, 3.000000000000000888 ) ) ;
#9351 = SHAPE_DEFINITION_REPRESENTATION ( #11592, #1997 ) ;
#9352 = CARTESIAN_POINT ( 'NONE',  ( 66.19999999999998863, 90.00000000000000000, 3.537500001229034297 ) ) ;
#9353 = ORIENTED_EDGE ( 'NONE', *, *, #200, .F. ) ;
#9354 = CARTESIAN_POINT ( 'NONE',  ( 65.00000000000000000, 117.5000000000001705, -0.9999999999999970024 ) ) ;
#9355 = ADVANCED_FACE ( 'NONE', ( #9168 ), #4143, .F. ) ;
#9356 = ORIENTED_EDGE ( 'NONE', *, *, #1139, .T. ) ;
#9357 = EDGE_CURVE ( 'NONE', #3419, #2347, #12314, .T. ) ;
#9358 = FACE_OUTER_BOUND ( 'NONE', #10930, .T. ) ;
#9359 = VECTOR ( 'NONE', #5302, 1000.000000000000000 ) ;
#9360 = DIRECTION ( 'NONE',  ( 1.000000000000000000, 0.000000000000000000, 0.000000000000000000 ) ) ;
#9361 = DIRECTION ( 'NONE',  ( 1.000000000000000000, 0.000000000000000000, 0.000000000000000000 ) ) ;
#9362 = ORIENTED_EDGE ( 'NONE', *, *, #9052, .F. ) ;
#9363 = DIRECTION ( 'NONE',  ( -0.9396926073018736503, -0.3420201803727477285, 0.000000000000000000 ) ) ;
#9364 = VERTEX_POINT ( 'NONE', #11200 ) ;
#9365 = VECTOR ( 'NONE', #5923, 1000.000000000000000 ) ;
#9366 = DIRECTION ( 'NONE',  ( 0.000000000000000000, 0.000000000000000000, -1.000000000000000000 ) ) ;
#9367 = VECTOR ( 'NONE', #11496, 1000.000000000000000 ) ;
#9368 = CARTESIAN_POINT ( 'NONE',  ( 3.556430356250028790, 71.84604660189818048, 3.996875000614517059 ) ) ;
#9369 = ORIENTED_EDGE ( 'NONE', *, *, #11585, .T. ) ;
#9370 = CARTESIAN_POINT ( 'NONE',  ( -18.33333333333332504, 30.00000000000000000, -7.999999999999996447 ) ) ;
#9371 = DIRECTION ( 'NONE',  ( -1.000000000000000000, 0.000000000000000000, 0.000000000000000000 ) ) ;
#9372 = CARTESIAN_POINT ( 'NONE',  ( 4.336808689942017736E-16, 0.000000000000000000, 0.000000000000000000 ) ) ;
#9373 = LINE ( 'NONE', #7350, #4967 ) ;
#9374 = EDGE_CURVE ( 'NONE', #5809, #9809, #8353, .T. ) ;
#9376 = AXIS2_PLACEMENT_3D ( 'NONE', #4222, #12193, #8337 ) ;
#9375 = CARTESIAN_POINT ( 'NONE',  ( 35.75000000000000711, 93.41869858279433458, -3.000000000000000000 ) ) ;
#9377 = CARTESIAN_POINT ( 'NONE',  ( 35.00000000000000000, 90.00000000000000000, -5.000000000000000000 ) ) ;
#9378 = CARTESIAN_POINT ( 'NONE',  ( 25.00000000000000355, 2.000000000000001332, -5.750000000000000000 ) ) ;
#9379 = DIRECTION ( 'NONE',  ( -0.000000000000000000, -0.000000000000000000, -1.000000000000000000 ) ) ;
#9380 = CARTESIAN_POINT ( 'NONE',  ( 48.49999999999995737, 90.00000000000000000, -8.000000000000000000 ) ) ;
#9381 = AXIS2_PLACEMENT_3D ( 'NONE', #5743, #4768, #10840 ) ;
#9382 = CARTESIAN_POINT ( 'NONE',  ( -53.07079676972452376, 33.99826794919245998, -1.000000000000000000 ) ) ;
#9383 = AXIS2_PLACEMENT_3D ( 'NONE', #3096, #7075, #2110 ) ;
#9384 = DIRECTION ( 'NONE',  ( 0.03100775193798453039, -0.9995191440486532741, 0.000000000000000000 ) ) ;
#9385 = CARTESIAN_POINT ( 'NONE',  ( 3.799999999999985612, 108.0133283987162827, 3.725000001229034741 ) ) ;
#9386 = VERTEX_POINT ( 'NONE', #8132 ) ;
#9387 = DIRECTION ( 'NONE',  ( -0.000000000000000000, -0.000000000000000000, -1.000000000000000000 ) ) ;
#9388 = DIRECTION ( 'NONE',  ( -0.000000000000000000, -0.000000000000000000, -1.000000000000000000 ) ) ;
#9389 = EDGE_LOOP ( 'NONE', ( #7023, #9860, #2051, #7495 ) ) ;
#9390 = EDGE_CURVE ( 'NONE', #12128, #11833, #9391, .T. ) ;
#9391 = CIRCLE ( 'NONE', #8146, 1.599999999999997202 ) ;
#9392 = CARTESIAN_POINT ( 'NONE',  ( 35.00000000000000000, 90.00000000000000000, -5.000000000000000000 ) ) ;
#9393 = DIRECTION ( 'NONE',  ( 1.000000000000000000, 0.000000000000000000, -0.000000000000000000 ) ) ;
#9394 = DIRECTION ( 'NONE',  ( -0.000000000000000000, -1.000000000000000000, 0.000000000000000000 ) ) ;
#9395 = ORIENTED_EDGE ( 'NONE', *, *, #7547, .T. ) ;
#9396 = CARTESIAN_POINT ( 'NONE',  ( 48.49999999999995737, 90.00000000000000000, -8.000000000000000000 ) ) ;
#9397 = DIRECTION ( 'NONE',  ( 1.000000000000000000, 0.000000000000000000, 0.000000000000000000 ) ) ;
#9398 = ORIENTED_EDGE ( 'NONE', *, *, #3554, .F. ) ;
#9399 = AXIS2_PLACEMENT_3D ( 'NONE', #4433, #3330, #12546 ) ;
#9400 =( NAMED_UNIT ( * ) SI_UNIT ( $, .STERADIAN. ) SOLID_ANGLE_UNIT ( ) );
#9401 = ORIENTED_EDGE ( 'NONE', *, *, #3904, .F. ) ;
#9402 = EDGE_CURVE ( 'NONE', #11453, #5904, #10219, .T. ) ;
#9403 = VERTEX_POINT ( 'NONE', #5180 ) ;
#9404 = DIRECTION ( 'NONE',  ( -1.000000000000000000, 0.000000000000000000, -0.000000000000000000 ) ) ;
#9405 = LINE ( 'NONE', #2547, #10829 ) ;
#9406 = ORIENTED_EDGE ( 'NONE', *, *, #7915, .T. ) ;
#9407 = VECTOR ( 'NONE', #3251, 1000.000000000000000 ) ;
#9408 = AXIS2_PLACEMENT_3D ( 'NONE', #697, #1629, #6786 ) ;
#9409 = EDGE_LOOP ( 'NONE', ( #12644, #12345, #1305, #12010 ) ) ;
#9410 = LINE ( 'NONE', #3536, #1789 ) ;
#9411 = ORIENTED_EDGE ( 'NONE', *, *, #11395, .F. ) ;
#9412 = CARTESIAN_POINT ( 'NONE',  ( 31.93836427709092973, 121.3209901524069636, 3.000000000000000444 ) ) ;
#9413 = ITEM_DEFINED_TRANSFORMATION ( 'NONE', 'NONE', #1332,  #5704 ) ;
#9414 = CARTESIAN_POINT ( 'NONE',  ( 3.799999999999904787, 71.98667160128373155, 3.237499999999999822 ) ) ;
#9415 = ORIENTED_EDGE ( 'NONE', *, *, #3609, .T. ) ;
#9416 = CARTESIAN_POINT ( 'NONE',  ( 35.00000000000000000, 90.00000000000000000, -8.000000000000000000 ) ) ;
#9417 = ORIENTED_EDGE ( 'NONE', *, *, #8901, .F. ) ;
#9418 = EDGE_CURVE ( 'NONE', #10216, #9176, #192, .T. ) ;
#9419 = CIRCLE ( 'NONE', #10040, 1.424999999999999822 ) ;
#9420 = CARTESIAN_POINT ( 'NONE',  ( 41.46432142674534305, 60.70473504998254555, -0.9999999999999970024 ) ) ;
#9421 = EDGE_LOOP ( 'NONE', ( #4683, #3870, #12884, #11677, #8509 ) ) ;
#9422 = CARTESIAN_POINT ( 'NONE',  ( 1.649999999999999911, 0.000000000000000000, 0.000000000000000000 ) ) ;
#9423 = DIRECTION ( 'NONE',  ( -1.000000000000000000, 0.000000000000000000, -0.000000000000000000 ) ) ;
#9424 =( LENGTH_UNIT ( ) NAMED_UNIT ( * ) SI_UNIT ( .MILLI., .METRE. ) );
#9425 = EDGE_CURVE ( 'NONE', #10649, #4500, #3232, .T. ) ;
#9427 = ADVANCED_FACE ( 'NONE', ( #4209 ), #7340, .F. ) ;
#9426 = EDGE_LOOP ( 'NONE', ( #2435, #9683, #11655, #1161 ) ) ;
#9428 = CIRCLE ( 'NONE', #10682, 0.1000000000000000472 ) ;
#9429 = CARTESIAN_POINT ( 'NONE',  ( -0.1038759689922479496, -3.348389132562988646, -0.8000000000000000444 ) ) ;
#9430 = CARTESIAN_POINT ( 'NONE',  ( -16.33333333333332504, 46.12451549659709116, 7.999999999999996447 ) ) ;
#9431 = CARTESIAN_POINT ( 'NONE',  ( 3.556430356250014579, 108.1539533981018053, 3.021875000614517415 ) ) ;
#9432 = ORIENTED_EDGE ( 'NONE', *, *, #11576, .F. ) ;
#9433 = PLANE ( 'NONE',  #7329 ) ;
#9434 = EDGE_CURVE ( 'NONE', #5827, #8056, #2315, .T. ) ;
#9435 = PLANE ( 'NONE',  #5780 ) ;
#9436 = CARTESIAN_POINT ( 'NONE',  ( 35.00000000000000711, 53.69209320379639649, 4.521875000614516971 ) ) ;
#9437 = VECTOR ( 'NONE', #7052, 1000.000000000000000 ) ;
#9438 = CARTESIAN_POINT ( 'NONE',  ( 50.72178482187499071, 117.2309300971526937, 4.653125000614517504 ) ) ;
#9439 = CARTESIAN_POINT ( 'NONE',  ( 60.00000000000000000, -6.000000000000000000, -15.00000000000000355 ) ) ;
#9440 =( BOUNDED_CURVE ( )  B_SPLINE_CURVE ( 2, ( #11448, #11384, #3291, #3415, #7205, #3355, #1308 ),
 .UNSPECIFIED., .F., .F. ) 
 B_SPLINE_CURVE_WITH_KNOTS ( ( 3, 2, 2, 3 ),
 ( 0.1000000000000001860, 0.1333333333333334425, 0.1666666666666666852, 0.2000000000000000111 ),
 .UNSPECIFIED. ) 
 CURVE ( )  GEOMETRIC_REPRESENTATION_ITEM ( )  RATIONAL_B_SPLINE_CURVE ( ( 0.9999999999999992228, 0.8660254037844394848, 1.000000000000000000, 0.8660254037844387076, 1.000000000000000000, 0.8660254037844388186, 0.9999999999999998890 ) ) 
 REPRESENTATION_ITEM ( '' )  );
#9441 = CARTESIAN_POINT ( 'NONE',  ( -6.666666666666660745, -5.000000000000000000, -1.499999999999999556 ) ) ;
#9442 = ADVANCED_FACE ( 'NONE', ( #10080, #6290 ), #4336, .F. ) ;
#9443 = CARTESIAN_POINT ( 'NONE',  ( 13.95244456248789788, 109.9499476216067819, -1.000000000000000000 ) ) ;
#9444 = DIRECTION ( 'NONE',  ( 0.8660254037844361541, 0.5000000000000042188, 0.000000000000000000 ) ) ;
#9445 = LINE ( 'NONE', #8662, #3664 ) ;
#9446 = CIRCLE ( 'NONE', #11107, 4.338286831716297698 ) ;
#9447 = LINE ( 'NONE', #6498, #5762 ) ;
#9448 = CARTESIAN_POINT ( 'NONE',  ( 3.800000000000015810, 108.0133283987162969, 4.962499999999999467 ) ) ;
#9449 = DIRECTION ( 'NONE',  ( 0.000000000000000000, 0.000000000000000000, -1.000000000000000000 ) ) ;
#9450 = ORIENTED_EDGE ( 'NONE', *, *, #3048, .F. ) ;
#9451 = DIRECTION ( 'NONE',  ( 1.000000000000000000, 0.000000000000000000, 0.000000000000000000 ) ) ;
#9452 = DIRECTION ( 'NONE',  ( -1.000000000000000000, 0.000000000000000000, 0.000000000000000000 ) ) ;
#9453 = ORIENTED_EDGE ( 'NONE', *, *, #10848, .T. ) ;
#9454 = AXIS2_PLACEMENT_3D ( 'NONE', #9078, #106, #12817 ) ;
#9455 = PLANE ( 'NONE',  #5930 ) ;
#9456 = LINE ( 'NONE', #1853, #5764 ) ;
#9457 = FACE_BOUND ( 'NONE', #7700, .T. ) ;
#9458 = ORIENTED_EDGE ( 'NONE', *, *, #9473, .F. ) ;
#9459 = CARTESIAN_POINT ( 'NONE',  ( -1.625004804578467077, -6.241943558307533557, -0.8000000000000000444 ) ) ;
#9460 = EDGE_CURVE ( 'NONE', #6459, #6839, #1314, .T. ) ;
#9461 = CARTESIAN_POINT ( 'NONE',  ( 66.44356964374999563, 90.00000000000000000, 4.578125000614516438 ) ) ;
#9462 = VERTEX_POINT ( 'NONE', #327 ) ;
#9463 = PRESENTATION_LAYER_ASSIGNMENT (  '', '', ( #9040 ) ) ;
#9464 = LINE ( 'NONE', #10384, #9112 ) ;
#9465 = ORIENTED_EDGE ( 'NONE', *, *, #10006, .F. ) ;
#9466 = CARTESIAN_POINT ( 'NONE',  ( 9.999999999999994671, 30.00000000000000000, -2.500000000000000000 ) ) ;
#9467 = VERTEX_POINT ( 'NONE', #8327 ) ;
#9468 = VECTOR ( 'NONE', #10961, 1000.000000000000000 ) ;
#9469 = CARTESIAN_POINT ( 'NONE',  ( 35.00000000000000000, 90.00000000000000000, 4.000000000000000000 ) ) ;
#9470 = CARTESIAN_POINT ( 'NONE',  ( 35.49999999999993605, 122.5000000000000142, 1.000000000000003109 ) ) ;
#9471 = VERTEX_POINT ( 'NONE', #1255 ) ;
#9472 =( GEOMETRIC_REPRESENTATION_CONTEXT ( 3 ) GLOBAL_UNCERTAINTY_ASSIGNED_CONTEXT ( ( #1193 ) ) GLOBAL_UNIT_ASSIGNED_CONTEXT ( ( #9138, #11954, #31 ) ) REPRESENTATION_CONTEXT ( 'NONE', 'WORKASPACE' ) );
#9473 = EDGE_CURVE ( 'NONE', #11514, #8561, #12052, .T. ) ;
#9474 = EDGE_LOOP ( 'NONE', ( #2087, #4424, #5098, #11071 ) ) ;
#9475 = CARTESIAN_POINT ( 'NONE',  ( 35.00000000000000000, 90.00000000000000000, 5.000000000000000000 ) ) ;
#9476 = ORIENTED_EDGE ( 'NONE', *, *, #4971, .T. ) ;
#9477 = VECTOR ( 'NONE', #2341, 1000.000000000000000 ) ;
#9478 = DIRECTION ( 'NONE',  ( 1.000000000000000000, 0.000000000000000000, 0.000000000000000000 ) ) ;
#9479 = EDGE_CURVE ( 'NONE', #10380, #4511, #3345, .T. ) ;
#9480 = CARTESIAN_POINT ( 'NONE',  ( 66.19999999999998863, 90.00000000000000000, 4.437500001229033764 ) ) ;
#9481 = ORIENTED_EDGE ( 'NONE', *, *, #6361, .F. ) ;
#9482 = DIRECTION ( 'NONE',  ( -0.000000000000000000, -0.000000000000000000, 1.000000000000000000 ) ) ;
#9483 = ORIENTED_EDGE ( 'NONE', *, *, #11995, .T. ) ;
#9484 = EDGE_CURVE ( 'NONE', #5315, #1634, #7041, .T. ) ;
#9485 = LINE ( 'NONE', #3544, #4004 ) ;
#9486 = ORIENTED_EDGE ( 'NONE', *, *, #2143, .T. ) ;
#9487 = CARTESIAN_POINT ( 'NONE',  ( 45.00000000000000000, 2.000000000000001332, -5.750000000000000000 ) ) ;
#9488 = PLANE ( 'NONE',  #8733 ) ;
#9489 = VECTOR ( 'NONE', #5324, 1000.000000000000114 ) ;
#9490 = UNCERTAINTY_MEASURE_WITH_UNIT (LENGTH_MEASURE( 1.000000000000000082E-05 ), #9260, 'distance_accuracy_value', 'NONE');
#9491=STYLED_ITEM('',(#13016),#7850);
#9492 = EDGE_CURVE ( 'NONE', #2828, #8136, #10611, .T. ) ;
#9493 = EDGE_LOOP ( 'NONE', ( #724, #9617, #6893, #10266 ) ) ;
#9494 = CARTESIAN_POINT ( 'NONE',  ( 19.27821517812500574, 117.2309300971526937, 4.728125000614516793 ) ) ;
#9495 = CARTESIAN_POINT ( 'NONE',  ( 66.44356964374998142, 108.1539533981018053, 3.321875000614517237 ) ) ;
#9496 = ORIENTED_EDGE ( 'NONE', *, *, #11511, .F. ) ;
#9497 = DIRECTION ( 'NONE',  ( -1.000000000000000000, -0.000000000000000000, -0.000000000000000000 ) ) ;
#9498 = ORIENTED_EDGE ( 'NONE', *, *, #8313, .T. ) ;
#9499 = AXIS2_PLACEMENT_3D ( 'NONE', #10812, #7802, #12658 ) ;
#9500 = CARTESIAN_POINT ( 'NONE',  ( 19.27821517812500574, 117.2309300971526937, 4.784375000614516260 ) ) ;
#9501 = PRODUCT_DEFINITION_SHAPE ( 'NONE', 'NONE',  #12586 ) ;
#9502 = ORIENTED_EDGE ( 'NONE', *, *, #8910, .F. ) ;
#9503 = DIRECTION ( 'NONE',  ( 0.000000000000000000, 0.000000000000000000, 1.000000000000000000 ) ) ;
#9504 = CARTESIAN_POINT ( 'NONE',  ( 4.995430082848484332, 99.45808535391196870, 2.999999999999999112 ) ) ;
#9505 = FACE_OUTER_BOUND ( 'NONE', #10206, .T. ) ;
#9506 = DIRECTION ( 'NONE',  ( 0.000000000000000000, 0.000000000000000000, 1.000000000000000000 ) ) ;
#9507 = CYLINDRICAL_SURFACE ( 'NONE', #12925, 1.599999999999992095 ) ;
#9508 = CIRCLE ( 'NONE', #7212, 4.000000000000003553 ) ;
#9509 = LINE ( 'NONE', #4541, #6665 ) ;
#9510 = AXIS2_PLACEMENT_3D ( 'NONE', #8694, #10781, #10651 ) ;
#9511 = DIRECTION ( 'NONE',  ( 0.000000000000000000, 0.000000000000000000, 1.000000000000000000 ) ) ;
#9512 = PLANE ( 'NONE',  #8762 ) ;
#9513 = DIRECTION ( 'NONE',  ( 0.000000000000000000, 0.000000000000000000, 1.000000000000000000 ) ) ;
#9514 = DIRECTION ( 'NONE',  ( -1.000000000000000000, -0.000000000000000000, -0.000000000000000000 ) ) ;
#9515 = CARTESIAN_POINT ( 'NONE',  ( -9.666666666666657193, 59.05996354921150271, -1.000000000000000222 ) ) ;
#9516 = AXIS2_PLACEMENT_3D ( 'NONE', #7616, #9514, #12659 ) ;
#9517 = LINE ( 'NONE', #7618, #5979 ) ;
#9519 = ADVANCED_FACE ( 'NONE', ( #11391, #6612 ), #389, .F. ) ;
#9518 = ORIENTED_EDGE ( 'NONE', *, *, #3965, .T. ) ;
#9520 = EDGE_CURVE ( 'NONE', #4578, #1698, #3559, .T. ) ;
#9521 = CIRCLE ( 'NONE', #1162, 1.500000000000001332 ) ;
#9522 = CARTESIAN_POINT ( 'NONE',  ( 35.00000000000000000, 90.00000000000000000, -0.9999999999999970024 ) ) ;
#9523 = SHAPE_REPRESENTATION ( 'socket button head screw_iso_ISO 7380 - M3 x 6 - 6N', ( #5704 ), #12825 ) ;
#9524 = CARTESIAN_POINT ( 'NONE',  ( 43.71630314554308683, 62.34089554097971586, -0.9999999999999970024 ) ) ;
#9525 = VERTEX_POINT ( 'NONE', #8392 ) ;
#9526 = LINE ( 'NONE', #8484, #10738 ) ;
#9527 = DIRECTION ( 'NONE',  ( -0.000000000000000000, -0.000000000000000000, -1.000000000000000000 ) ) ;
#9528 = AXIS2_PLACEMENT_3D ( 'NONE', #4928, #8915, #8726 ) ;
#9529 = DIRECTION ( 'NONE',  ( -0.000000000000000000, -0.000000000000000000, -1.000000000000000000 ) ) ;
#9530 = AXIS2_PLACEMENT_3D ( 'NONE', #6920, #9929, #6857 ) ;
#9531 = ORIENTED_EDGE ( 'NONE', *, *, #2605, .T. ) ;
#9532 = FACE_OUTER_BOUND ( 'NONE', #9255, .T. ) ;
#9533 = CYLINDRICAL_SURFACE ( 'NONE', #8778, 1.599999999999990319 ) ;
#9534 = ORIENTED_EDGE ( 'NONE', *, *, #5737, .T. ) ;
#9535 = CARTESIAN_POINT ( 'NONE',  ( 0.000000000000000000, 0.000000000000000000, 0.000000000000000000 ) ) ;
#9536 = CARTESIAN_POINT ( 'NONE',  ( 5.000000000000004441, 76.58915998087155685, 2.500000000000000444 ) ) ;
#9537 = VERTEX_POINT ( 'NONE', #5499 ) ;
#9538 = DIRECTION ( 'NONE',  ( -0.000000000000000000, -1.000000000000000000, -0.000000000000000000 ) ) ;
#9539 = ORIENTED_EDGE ( 'NONE', *, *, #2241, .F. ) ;
#9540 = VECTOR ( 'NONE', #12322, 1000.000000000000000 ) ;
#9541 = DIRECTION ( 'NONE',  ( 0.000000000000000000, 0.000000000000000000, -1.000000000000000000 ) ) ;
#9542 = DIRECTION ( 'NONE',  ( 3.497202527569242313E-15, -1.000000000000000000, 0.000000000000000000 ) ) ;
#9543 = EDGE_CURVE ( 'NONE', #11641, #4459, #6546, .T. ) ;
#9544 = ORIENTED_EDGE ( 'NONE', *, *, #2258, .F. ) ;
#9545 = CARTESIAN_POINT ( 'NONE',  ( 35.00000000000000000, 90.00000000000000000, 6.000000000000000000 ) ) ;
#9546 = ORIENTED_EDGE ( 'NONE', *, *, #3194, .T. ) ;
#9547 = CARTESIAN_POINT ( 'NONE',  ( 35.49999999999995026, 119.9958330439412890, -3.000000000000000000 ) ) ;
#9548 = ORIENTED_EDGE ( 'NONE', *, *, #11025, .F. ) ;
#9549 = PLANE ( 'NONE',  #12005 ) ;
#9550 = CARTESIAN_POINT ( 'NONE',  ( 19.40000000000002700, 62.98000740192551206, 3.275000000000000355 ) ) ;
#9551 = VECTOR ( 'NONE', #4135, 1000.000000000000000 ) ;
#9552 = ORIENTED_EDGE ( 'NONE', *, *, #739, .F. ) ;
#9553 = ORIENTED_EDGE ( 'NONE', *, *, #5485, .T. ) ;
#9554 = EDGE_CURVE ( 'NONE', #3214, #7217, #6416, .T. ) ;
#9555 = FACE_OUTER_BOUND ( 'NONE', #3913, .T. ) ;
#9556 = ORIENTED_EDGE ( 'NONE', *, *, #7447, .T. ) ;
#9557 = CARTESIAN_POINT ( 'NONE',  ( 15.79116220520106495, 65.24871774101997346, 3.000000000000002220 ) ) ;
#9558 = DIRECTION ( 'NONE',  ( 0.000000000000000000, 0.000000000000000000, 1.000000000000000000 ) ) ;
#9559 = ADVANCED_FACE ( 'NONE', ( #7599 ), #588, .F. ) ;
#9560 = TOROIDAL_SURFACE ( 'NONE', #350, 1.599999999999998757, 0.1000000000000000056 ) ;
#9561 = ORIENTED_EDGE ( 'NONE', *, *, #6736, .T. ) ;
#9562 = DIRECTION ( 'NONE',  ( 0.000000000000000000, 0.000000000000000000, -1.000000000000000000 ) ) ;
#9563 = ORIENTED_EDGE ( 'NONE', *, *, #3846, .T. ) ;
#9564 = CARTESIAN_POINT ( 'NONE',  ( 66.19999999999998863, 90.00000000000000000, 3.087500001229034119 ) ) ;
#9565 = ORIENTED_EDGE ( 'NONE', *, *, #1250, .F. ) ;
#9566 = CARTESIAN_POINT ( 'NONE',  ( 19.27821517812500574, 117.2309300971526937, 3.884375000614516793 ) ) ;
#9567 = EDGE_LOOP ( 'NONE', ( #687, #6356, #10569 ) ) ;
#9568 = FACE_OUTER_BOUND ( 'NONE', #3716, .T. ) ;
#9569 = CARTESIAN_POINT ( 'NONE',  ( 1.040000000000000036, -0.5773502691896255090, 1.000000000000000000 ) ) ;
#9570 = EDGE_CURVE ( 'NONE', #6259, #8071, #1449, .T. ) ;
#9571 = CARTESIAN_POINT ( 'NONE',  ( 33.90709641728108892, 93.16671150547063007, 4.800000000000000711 ) ) ;
#9572 = CARTESIAN_POINT ( 'NONE',  ( 25.00000000000000355, 0.000000000000000000, -5.750000000000000000 ) ) ;
#9573 = DIRECTION ( 'NONE',  ( -0.000000000000000000, -0.000000000000000000, -1.000000000000000000 ) ) ;
#9574 = DIRECTION ( 'NONE',  ( 1.000000000000000000, 0.000000000000000000, 0.000000000000000000 ) ) ;
#9575 = VECTOR ( 'NONE', #1391, 1000.000000000000000 ) ;
#9576 = FACE_OUTER_BOUND ( 'NONE', #10847, .T. ) ;
#9577 = LINE ( 'NONE', #5713, #4374 ) ;
#9578 = DIRECTION ( 'NONE',  ( -0.000000000000000000, 0.000000000000000000, 1.000000000000000000 ) ) ;
#9579 = DIRECTION ( 'NONE',  ( 0.1305261922200528224, -0.9914448613738103822, 0.000000000000000000 ) ) ;
#9580 = CARTESIAN_POINT ( 'NONE',  ( -9.666666666666657193, 61.36936462597000741, 3.000000000000059508 ) ) ;
#9581 = CARTESIAN_POINT ( 'NONE',  ( 66.19999999999998863, 90.00000000000000000, 5.000000000000000000 ) ) ;
#9582 = ORIENTED_EDGE ( 'NONE', *, *, #4123, .T. ) ;
#9583 = EDGE_CURVE ( 'NONE', #5750, #9165, #295, .T. ) ;
#9584 = AXIS2_PLACEMENT_3D ( 'NONE', #2155, #3995, #4119 ) ;
#9585 = CARTESIAN_POINT ( 'NONE',  ( 66.19999999999998863, 90.00000000000000000, 3.875000000000000000 ) ) ;
#9586 = LINE ( 'NONE', #1671, #4958 ) ;
#9587 = ORIENTED_EDGE ( 'NONE', *, *, #666, .F. ) ;
#9588 = FILL_AREA_STYLE ('',( #5596 ) ) ;
#9589 = DIRECTION ( 'NONE',  ( -0.000000000000000000, 1.000000000000000000, -0.000000000000000000 ) ) ;
#9590 = ADVANCED_FACE ( 'NONE', ( #4595 ), #2635, .T. ) ;
#9591 = CIRCLE ( 'NONE', #11673, 6.450000000000001066 ) ;
#9592 = ADVANCED_FACE ( 'NONE', ( #10670 ), #8589, .T. ) ;
#9593 = ORIENTED_EDGE ( 'NONE', *, *, #2993, .T. ) ;
#9594 = FACE_OUTER_BOUND ( 'NONE', #1546, .T. ) ;
#9595 = CARTESIAN_POINT ( 'NONE',  ( 50.72178482187501203, 62.76906990284730625, 3.153125000614517504 ) ) ;
#9596 = ORIENTED_EDGE ( 'NONE', *, *, #6031, .F. ) ;
#9597 = LINE ( 'NONE', #12674, #5437 ) ;
#9598 = CARTESIAN_POINT ( 'NONE',  ( -57.99999999999999289, 2.000000000000000000, 0.000000000000000000 ) ) ;
#9599 = ORIENTED_EDGE ( 'NONE', *, *, #4872, .T. ) ;
#9600 = CIRCLE ( 'NONE', #7301, 1.499999999999999556 ) ;
#9601 = CARTESIAN_POINT ( 'NONE',  ( 66.19999999999998863, 90.00000000000000000, 5.000000000000000000 ) ) ;
#9602 = VERTEX_POINT ( 'NONE', #8649 ) ;
#9603 = EDGE_CURVE ( 'NONE', #5282, #4450, #8754, .T. ) ;
#9604 = AXIS2_PLACEMENT_3D ( 'NONE', #6494, #6558, #534 ) ;
#9605 = CARTESIAN_POINT ( 'NONE',  ( -28.99038105676692112, 50.21281292110204930, 0.000000000000000000 ) ) ;
#9606 = LINE ( 'NONE', #11755, #5625 ) ;
#9607 = CARTESIAN_POINT ( 'NONE',  ( -4.270088556250601699E-16, 2.000000000000000000, 8.000000000000000000 ) ) ;
#9608 = EDGE_LOOP ( 'NONE', ( #6142, #7867, #12502, #6919, #475 ) ) ;
#9609 = CARTESIAN_POINT ( 'NONE',  ( 25.00000000000000355, 2.000000000000000000, 7.349999999999991651 ) ) ;
#9610 = ORIENTED_EDGE ( 'NONE', *, *, #10709, .T. ) ;
#9611 = DIRECTION ( 'NONE',  ( -0.000000000000000000, -0.000000000000000000, -1.000000000000000000 ) ) ;
#9612 = APPLICATION_PROTOCOL_DEFINITION ( 'draft international standard', 'automotive_design', 1998, #2515 ) ;
#9613 = CARTESIAN_POINT ( 'NONE',  ( 19.40000000000000924, 117.0199925980744666, 2.787500001229034297 ) ) ;
#9614 = EDGE_LOOP ( 'NONE', ( #2570, #1704, #5288, #6502 ) ) ;
#9615 = EDGE_CURVE ( 'NONE', #955, #10005, #3686, .T. ) ;
#9616 =( NAMED_UNIT ( * ) PLANE_ANGLE_UNIT ( ) SI_UNIT ( $, .RADIAN. ) );
#9617 = ORIENTED_EDGE ( 'NONE', *, *, #1675, .T. ) ;
#9618 =( NAMED_UNIT ( * ) SI_UNIT ( $, .STERADIAN. ) SOLID_ANGLE_UNIT ( ) );
#9619 = ORIENTED_EDGE ( 'NONE', *, *, #9434, .F. ) ;
#9620 = CARTESIAN_POINT ( 'NONE',  ( 39.18799846562198042, 59.03019923891626064, 3.000000000000000000 ) ) ;
#9621 = CIRCLE ( 'NONE', #3982, 28.99999999999999289 ) ;
#9622 = CARTESIAN_POINT ( 'NONE',  ( -60.00000000000000000, 30.00000000000000000, 9.999999999999996447 ) ) ;
#9623 = UNCERTAINTY_MEASURE_WITH_UNIT (LENGTH_MEASURE( 1.000000000000000082E-05 ), #10017, 'distance_accuracy_value', 'NONE');
#9624 = ORIENTED_EDGE ( 'NONE', *, *, #11067, .T. ) ;
#9625 = CARTESIAN_POINT ( 'NONE',  ( 66.44356964374999563, 71.84604660189820891, 4.146875000614517859 ) ) ;
#9626 = EDGE_CURVE ( 'NONE', #9895, #11248, #6483, .T. ) ;
#9627 = VERTEX_POINT ( 'NONE', #7535 ) ;
#9628 = DIRECTION ( 'NONE',  ( -0.000000000000000000, -0.000000000000000000, 1.000000000000000000 ) ) ;
#9629 = ORIENTED_EDGE ( 'NONE', *, *, #6990, .T. ) ;
#9630 = CARTESIAN_POINT ( 'NONE',  ( 66.44356964374998142, 108.1539533981018053, 4.671875000614516438 ) ) ;
#9631 = EDGE_CURVE ( 'NONE', #3765, #11967, #12538, .T. ) ;
#9632 = EDGE_LOOP ( 'NONE', ( #11558, #2342, #5522, #5249 ) ) ;
#9633 = PLANE ( 'NONE',  #6287 ) ;
#9634 = DIRECTION ( 'NONE',  ( 0.000000000000000000, 0.000000000000000000, 1.000000000000000000 ) ) ;
#9635 = CARTESIAN_POINT ( 'NONE',  ( 3.556430356250014579, 108.1539533981018053, 4.765625000614517326 ) ) ;
#9636 = AXIS2_PLACEMENT_3D ( 'NONE', #511, #6667, #646 ) ;
#9637 = DIRECTION ( 'NONE',  ( 0.000000000000000000, 0.000000000000000000, -1.000000000000000000 ) ) ;
#9638 = CARTESIAN_POINT ( 'NONE',  ( 35.00000000000000000, 90.00000000000000000, -3.000000000000000000 ) ) ;
#9639 = EDGE_CURVE ( 'NONE', #11453, #4275, #4850, .T. ) ;
#9640 = CARTESIAN_POINT ( 'NONE',  ( 25.00000000000000355, 0.000000000000000000, 4.150000000000003020 ) ) ;
#9641 = CARTESIAN_POINT ( 'NONE',  ( -36.66666666666665009, 30.00000000000000000, -7.999999999999996447 ) ) ;
#9642 = FACE_OUTER_BOUND ( 'NONE', #8646, .T. ) ;
#9643 = EDGE_CURVE ( 'NONE', #3461, #6695, #2891, .T. ) ;
#9644 = CIRCLE ( 'NONE', #2760, 28.99999999999999289 ) ;
#9645 = FACE_OUTER_BOUND ( 'NONE', #9852, .T. ) ;
#9646 = FACE_OUTER_BOUND ( 'NONE', #2037, .T. ) ;
#9647 = EDGE_LOOP ( 'NONE', ( #12215, #449, #12394, #8332 ) ) ;
#9648 = DIRECTION ( 'NONE',  ( 1.000000000000000000, 0.000000000000000000, 0.000000000000000000 ) ) ;
#9649 = ORIENTED_EDGE ( 'NONE', *, *, #3442, .T. ) ;
#9650 =( NAMED_UNIT ( * ) SI_UNIT ( $, .STERADIAN. ) SOLID_ANGLE_UNIT ( ) );
#9651 = CARTESIAN_POINT ( 'NONE',  ( 4.245171717594923066, 100.5185805753332033, 1.000000000000003109 ) ) ;
#9652 = EDGE_CURVE ( 'NONE', #6795, #11778, #817, .T. ) ;
#9653 = CARTESIAN_POINT ( 'NONE',  ( 35.00000000000000000, 90.00000000000000000, 8.000000000000000000 ) ) ;
#9654 = EDGE_LOOP ( 'NONE', ( #5611, #3605, #7574, #8860 ) ) ;
#9655 = LINE ( 'NONE', #8615, #7002 ) ;
#9656 = CARTESIAN_POINT ( 'NONE',  ( 19.27821517812503060, 62.76906990284727783, 3.978125000614516793 ) ) ;
#9657 = EDGE_CURVE ( 'NONE', #9462, #716, #12942, .T. ) ;
#9658 = CARTESIAN_POINT ( 'NONE',  ( 25.00000000000000355, 0.000000000000000000, -4.150000000000003020 ) ) ;
#9659 = CARTESIAN_POINT ( 'NONE',  ( 30.00000000000000711, 0.000000000000000000, -10.00000000000000000 ) ) ;
#9660 = VERTEX_POINT ( 'NONE', #1712 ) ;
#9661 = VECTOR ( 'NONE', #5376, 1000.000000000000000 ) ;
#9662 = CARTESIAN_POINT ( 'NONE',  ( 52.49999999999996447, 90.00000000000000000, -8.000000000000000000 ) ) ;
#9663 = EDGE_LOOP ( 'NONE', ( #7714, #5964, #9027, #6713 ) ) ;
#9664 = ADVANCED_FACE ( 'NONE', ( #4972 ), #10918, .T. ) ;
#9665 = DIRECTION ( 'NONE',  ( -0.000000000000000000, 0.000000000000000000, 1.000000000000000000 ) ) ;
#9666 = CARTESIAN_POINT ( 'NONE',  ( 0.000000000000000000, 0.000000000000000000, 2.849999999999999201 ) ) ;
#9667 = ORIENTED_EDGE ( 'NONE', *, *, #1409, .T. ) ;
#9668 = AXIS2_PLACEMENT_3D ( 'NONE', #3207, #5409, #9404 ) ;
#9669 = DIRECTION ( 'NONE',  ( -1.000000000000000000, 0.000000000000000000, -2.780005570475653612E-17 ) ) ;
#9670 = ORIENTED_EDGE ( 'NONE', *, *, #9473, .T. ) ;
#9671 = B_SPLINE_CURVE_WITH_KNOTS ( 'NONE', 3,
 ( #3679, #5629, #10470, #8766, #6731, #2561, #9620, #1705, #582, #5491, #4524, #12634, #3612, #6539, #1506, #2499, #8515, #11580, #3802, #9557, #648, #4587, #11645, #6669, #7781, #8580, #2757, #4717, #12573, #7720, #8703, #7591, #11708, #2629, #6604, #7531, #10723, #4779, #1640, #10537 ),
 .UNSPECIFIED., .F., .F.,
 ( 4, 2, 2, 2, 2, 2, 2, 2, 2, 2, 2, 2, 2, 2, 2, 2, 2, 2, 2, 4 ),
 ( 0.000000000000000000, 0.001930134362530089298, 0.003860268725060178596, 0.007720537450120362397, 0.01158080617518054620, 0.01544107490024072826, 0.02316161235036109586, 0.02509174671289119210, 0.02702188107542128834, 0.03088214980048148428, 0.03281228416301156664, 0.03474241852554164900, 0.03860268725060180678, 0.04053282161313188914, 0.04246295597566197150, 0.04632322470072212928, 0.05018349342578230093, 0.05404376215084246565, 0.05790403087590263037, 0.06176429960096278815 ),
 .UNSPECIFIED. ) ;
#9672 = LINE ( 'NONE', #5482, #10548 ) ;
#9673 = CARTESIAN_POINT ( 'NONE',  ( 35.00000000000000000, 90.00000000000000000, 22.38477631085024555 ) ) ;
#9674 = ORIENTED_EDGE ( 'NONE', *, *, #7629, .F. ) ;
#9675 = SURFACE_SIDE_STYLE ('',( #4648 ) ) ;
#9676 = VERTEX_POINT ( 'NONE', #11779 ) ;
#9677 =( LENGTH_UNIT ( ) NAMED_UNIT ( * ) SI_UNIT ( .MILLI., .METRE. ) );
#9678 = VERTEX_POINT ( 'NONE', #8832 ) ;
#9679 = EDGE_CURVE ( 'NONE', #703, #3473, #10858, .T. ) ;
#9680 = EDGE_CURVE ( 'NONE', #8908, #10536, #8562, .T. ) ;
#9681 = CARTESIAN_POINT ( 'NONE',  ( 21.49999999999998579, 90.00000000000000000, -5.000000000000000000 ) ) ;
#9682 = DIRECTION ( 'NONE',  ( -0.000000000000000000, -0.000000000000000000, -1.000000000000000000 ) ) ;
#9683 = ORIENTED_EDGE ( 'NONE', *, *, #3799, .F. ) ;
#9684 = CARTESIAN_POINT ( 'NONE',  ( 62.42406877266672183, 99.43633196372844907, 4.000000000000000000 ) ) ;
#9685 = ORIENTED_EDGE ( 'NONE', *, *, #3580, .F. ) ;
#9686 =( REPRESENTATION_RELATIONSHIP ('NONE','NONE', #1997, #9523 ) REPRESENTATION_RELATIONSHIP_WITH_TRANSFORMATION ( #9738 )SHAPE_REPRESENTATION_RELATIONSHIP( ) );
#9687 = DIRECTION ( 'NONE',  ( -0.000000000000000000, -1.000000000000000000, -0.000000000000000000 ) ) ;
#9688 = ORIENTED_EDGE ( 'NONE', *, *, #4684, .T. ) ;
#9689 = CARTESIAN_POINT ( 'NONE',  ( 3.556430356250015024, 90.00000000000000000, 3.903125000614517504 ) ) ;
#9690 = VERTEX_POINT ( 'NONE', #6738 ) ;
#9691 = DIRECTION ( 'NONE',  ( 1.000000000000000000, 2.135044278125301343E-15, 0.000000000000000000 ) ) ;
#9692 = AXIS2_PLACEMENT_3D ( 'NONE', #2279, #10310, #4239 ) ;
#9693 = CARTESIAN_POINT ( 'NONE',  ( 34.25000000000000000, 93.26496554346289258, -3.000000000000000000 ) ) ;
#9694 = SURFACE_STYLE_USAGE ( .BOTH. , #5707 ) ;
#9695 = CARTESIAN_POINT ( 'NONE',  ( 3.800000000000015365, 90.00000000000000000, 4.662500001229034297 ) ) ;
#9696 = AXIS2_PLACEMENT_3D ( 'NONE', #8062, #12046, #4267 ) ;
#9697 = CARTESIAN_POINT ( 'NONE',  ( 35.00000000000000000, 90.00000000000000000, 5.000000000000000000 ) ) ;
#9698 = EDGE_CURVE ( 'NONE', #3174, #4591, #12319, .T. ) ;
#9699 = CARTESIAN_POINT ( 'NONE',  ( 3.800000000000015365, 90.00000000000000000, 5.000000000000000000 ) ) ;
#9700 = AXIS2_PLACEMENT_3D ( 'NONE', #4751, #874, #937 ) ;
#9701 = LINE ( 'NONE', #11535, #807 ) ;
#9702 = CARTESIAN_POINT ( 'NONE',  ( 22.06359219780243208, 118.6456930160215251, 2.999999999999998668 ) ) ;
#9703 = CARTESIAN_POINT ( 'NONE',  ( 35.00000000000000000, 90.00000000000000000, 22.38477631085024555 ) ) ;
#9704 = LINE ( 'NONE', #740, #8172 ) ;
#9705 = CARTESIAN_POINT ( 'NONE',  ( 3.556430356250028790, 71.84604660189818048, 3.096875000614517592 ) ) ;
#9706 = ORIENTED_EDGE ( 'NONE', *, *, #3741, .F. ) ;
#9707 = CARTESIAN_POINT ( 'NONE',  ( 3.800000000000015365, 90.00000000000000000, 5.000000000000000000 ) ) ;
#9708 = ADVANCED_FACE ( 'NONE', ( #11715, #11845, #2952, #12766, #5884 ), #7787, .T. ) ;
#9709 = DIRECTION ( 'NONE',  ( 0.9347165045408831752, 0.3553942263724512163, 0.000000000000000000 ) ) ;
#9710 = EDGE_LOOP ( 'NONE', ( #1346, #9742, #12076, #2425, #7209, #3236, #6925, #11500, #8228, #3997, #7252, #2747 ) ) ;
#9711 = AXIS2_PLACEMENT_3D ( 'NONE', #5745, #3729, #7712 ) ;
#9712 = EDGE_CURVE ( 'NONE', #3747, #9191, #393, .T. ) ;
#9713 = AXIS2_PLACEMENT_3D ( 'NONE', #9378, #10561, #5648 ) ;
#9714 = EDGE_CURVE ( 'NONE', #870, #9327, #7984, .T. ) ;
#9715 = LINE ( 'NONE', #9780, #6769 ) ;
#9716 = LINE ( 'NONE', #1739, #8239 ) ;
#9717 = VECTOR ( 'NONE', #2876, 1000.000000000000000 ) ;
#9718 = PLANE ( 'NONE',  #4090 ) ;
#9719 = CARTESIAN_POINT ( 'NONE',  ( 66.44356964374998142, 108.1539533981018053, 4.165625000614516793 ) ) ;
#9720 = VECTOR ( 'NONE', #2950, 1000.000000000000000 ) ;
#9721 = LINE ( 'NONE', #4755, #11709 ) ;
#9722 = CARTESIAN_POINT ( 'NONE',  ( 9.369499999999998607, 0.000000000000000000, 1.500000000000000222 ) ) ;
#9723 = ORIENTED_EDGE ( 'NONE', *, *, #4458, .T. ) ;
#9724 = CYLINDRICAL_SURFACE ( 'NONE', #5576, 31.19999999999998863 ) ;
#9725 = EDGE_LOOP ( 'NONE', ( #9548, #11381, #4387, #10782, #10581 ) ) ;
#9726 = EDGE_CURVE ( 'NONE', #4212, #10418, #8959, .T. ) ;
#9727 = CARTESIAN_POINT ( 'NONE',  ( 66.19999999999998863, 90.00000000000000000, 3.987500001229034030 ) ) ;
#9728 = CYLINDRICAL_SURFACE ( 'NONE', #9999, 1.599999999999992095 ) ;
#9729 = AXIS2_PLACEMENT_3D ( 'NONE', #472, #404, #11668 ) ;
#9730 = CONICAL_SURFACE ( 'NONE', #1379, 1.500000000000001332, 1.029744260000000411 ) ;
#9731 = PRODUCT_DEFINITION_CONTEXT ( 'detailed design', #11442, 'design' ) ;
#9732 = LINE ( 'NONE', #3358, #3969 ) ;
#9733 = CARTESIAN_POINT ( 'NONE',  ( 1.040000000000000036, 0.5773502691896262862, 1.000000000000000000 ) ) ;
#9734 = ORIENTED_EDGE ( 'NONE', *, *, #2982, .F. ) ;
#9735 = CARTESIAN_POINT ( 'NONE',  ( 31.50000000000000000, 90.00000000000000000, 6.000000000000000000 ) ) ;
#9736 = ORIENTED_EDGE ( 'NONE', *, *, #705, .F. ) ;
#9737 = CARTESIAN_POINT ( 'NONE',  ( 3.800000000000015365, 90.00000000000000000, 5.000000000000000000 ) ) ;
#9738 = ITEM_DEFINED_TRANSFORMATION ( 'NONE', 'NONE', #11780,  #5704 ) ;
#9739 = CARTESIAN_POINT ( 'NONE',  ( -16.33333333333332504, 30.00000000000000000, 7.999999999999996447 ) ) ;
#9740 = VERTEX_POINT ( 'NONE', #3014 ) ;
#9741 = CYLINDRICAL_SURFACE ( 'NONE', #2227, 3.350000000000000089 ) ;
#9742 = ORIENTED_EDGE ( 'NONE', *, *, #10607, .T. ) ;
#9743 = PRESENTATION_LAYER_ASSIGNMENT (  '', '', ( #2860 ) ) ;
#9744 = FACE_OUTER_BOUND ( 'NONE', #7394, .T. ) ;
#9745 = ORIENTED_EDGE ( 'NONE', *, *, #9712, .T. ) ;
#9746 = EDGE_CURVE ( 'NONE', #376, #7167, #7000, .T. ) ;
#9747 = DIRECTION ( 'NONE',  ( 0.000000000000000000, 0.000000000000000000, 1.000000000000000000 ) ) ;
#9748 = DIRECTION ( 'NONE',  ( -0.000000000000000000, -0.000000000000000000, -1.000000000000000000 ) ) ;
#9749 = ORIENTED_EDGE ( 'NONE', *, *, #4858, .F. ) ;
#9750 = AXIS2_PLACEMENT_3D ( 'NONE', #9976, #5859, #1008 ) ;
#9751 = DIRECTION ( 'NONE',  ( -1.000000000000000000, -0.000000000000000000, -0.000000000000000000 ) ) ;
#9752 = ORIENTED_EDGE ( 'NONE', *, *, #4943, .T. ) ;
#9753 = EDGE_CURVE ( 'NONE', #7005, #3174, #11482, .T. ) ;
#9754 = DIRECTION ( 'NONE',  ( 0.000000000000000000, 0.000000000000000000, 1.000000000000000000 ) ) ;
#9755 = ADVANCED_FACE ( 'NONE', ( #719 ), #8710, .T. ) ;
#9756 = ORIENTED_EDGE ( 'NONE', *, *, #1293, .T. ) ;
#9757 = CARTESIAN_POINT ( 'NONE',  ( 3.556430356250028790, 71.84604660189818048, 4.390625000614517326 ) ) ;
#9758 = ORIENTED_EDGE ( 'NONE', *, *, #5314, .F. ) ;
#9759 = CARTESIAN_POINT ( 'NONE',  ( 6.499999999999999112, 70.70319397786906279, 2.999999999999960920 ) ) ;
#9760 = DIRECTION ( 'NONE',  ( -4.336808689942017243E-16, -2.503857664561960972E-16, -1.000000000000000000 ) ) ;
#9761 = VECTOR ( 'NONE', #5009, 999.9999999999998863 ) ;
#9762 = CARTESIAN_POINT ( 'NONE',  ( 72.83557806687970526, 62.54593364529978317, 1.000000000000003109 ) ) ;
#9763 = CARTESIAN_POINT ( 'NONE',  ( 19.27821517812500574, 117.2309300971526937, 2.928125000614517415 ) ) ;
#9764 = CARTESIAN_POINT ( 'NONE',  ( 1.040000000000000036, 0.000000000000000000, 2.000000000000000000 ) ) ;
#9765 = DIRECTION ( 'NONE',  ( -1.000000000000000000, -0.000000000000000000, -0.000000000000000000 ) ) ;
#9766 = DIRECTION ( 'NONE',  ( 1.000000000000000000, 0.000000000000000000, 0.000000000000000000 ) ) ;
#9767 = DIRECTION ( 'NONE',  ( -1.000000000000000000, 0.000000000000000000, -0.000000000000000000 ) ) ;
#9768 = FACE_OUTER_BOUND ( 'NONE', #2028, .T. ) ;
#9769 = AXIS2_PLACEMENT_3D ( 'NONE', #2854, #4938, #12853 ) ;
#9770 = FACE_OUTER_BOUND ( 'NONE', #720, .T. ) ;
#9771 = CARTESIAN_POINT ( 'NONE',  ( -60.00000000000000000, 30.00000000000000000, 3.000000000000000000 ) ) ;
#9772 = CARTESIAN_POINT ( 'NONE',  ( 60.63303222545420823, 111.5086687406912347, 2.885734441871016021 ) ) ;
#9773 = ADVANCED_FACE ( 'NONE', ( #5763 ), #10083, .T. ) ;
#9774 = ORIENTED_EDGE ( 'NONE', *, *, #3660, .T. ) ;
#9775 = CARTESIAN_POINT ( 'NONE',  ( 19.40000000000002700, 62.98000740192551206, 4.174999999999999822 ) ) ;
#9776 = CARTESIAN_POINT ( 'NONE',  ( 31.86869970978804290, 88.80942934165229019, 4.800000000000000711 ) ) ;
#9777 = EDGE_LOOP ( 'NONE', ( #5533, #11092, #9667, #8705 ) ) ;
#9778 = VECTOR ( 'NONE', #8704, 1000.000000000000000 ) ;
#9779 = SURFACE_SIDE_STYLE ('',( #1736 ) ) ;
#9780 = CARTESIAN_POINT ( 'NONE',  ( 3.000000000000004441, 2.000000000000000000, 0.000000000000000000 ) ) ;
#9781 = DIRECTION ( 'NONE',  ( -0.8660254037844361541, -0.5000000000000042188, 0.000000000000000000 ) ) ;
#9782 = EDGE_CURVE ( 'NONE', #10175, #1050, #1915, .T. ) ;
#9783 = CARTESIAN_POINT ( 'NONE',  ( 35.49951382533862443, 118.9974510565036070, 4.000000000000000000 ) ) ;
#9784 = CARTESIAN_POINT ( 'NONE',  ( 35.00000000000000711, 53.69209320379639649, 4.015625000614517326 ) ) ;
#9785 = VECTOR ( 'NONE', #9143, 1000.000000000000000 ) ;
#9786 = CARTESIAN_POINT ( 'NONE',  ( 44.20597631976078645, 117.5000000000000568, 1.000000000000003109 ) ) ;
#9787 = CARTESIAN_POINT ( 'NONE',  ( 35.00000000000000000, 126.3079067962036106, 4.746875000614517504 ) ) ;
#9788 = EDGE_CURVE ( 'NONE', #11574, #7460, #6836, .T. ) ;
#9789 = ORIENTED_EDGE ( 'NONE', *, *, #1841, .F. ) ;
#9790 = FACE_BOUND ( 'NONE', #1493, .T. ) ;
#9791 = EDGE_LOOP ( 'NONE', ( #4509, #773, #11643, #2275 ) ) ;
#9792 = DIRECTION ( 'NONE',  ( -5.624500927088228034E-17, 1.370729058197317775E-18, 1.000000000000000000 ) ) ;
#9793 = CARTESIAN_POINT ( 'NONE',  ( 0.1999999999999965694, -6.446898479113814417, -0.8000000000000000444 ) ) ;
#9794 = VECTOR ( 'NONE', #9290, 1000.000000000000000 ) ;
#9795 = DIRECTION ( 'NONE',  ( 0.000000000000000000, 0.000000000000000000, 1.000000000000000000 ) ) ;
#9796 = FACE_OUTER_BOUND ( 'NONE', #2855, .T. ) ;
#9797 = FACE_OUTER_BOUND ( 'NONE', #4970, .T. ) ;
#9798 = FACE_OUTER_BOUND ( 'NONE', #3863, .T. ) ;
#9799 = ORIENTED_EDGE ( 'NONE', *, *, #12163, .F. ) ;
#9800 = CYLINDRICAL_SURFACE ( 'NONE', #10962, 1.499999999999999556 ) ;
#9801 = DIRECTION ( 'NONE',  ( -1.000000000000000000, -2.081668171172168513E-14, 0.000000000000000000 ) ) ;
#9802 = EDGE_CURVE ( 'NONE', #7980, #3747, #507, .T. ) ;
#9803 = ORIENTED_EDGE ( 'NONE', *, *, #1171, .T. ) ;
#9804 = AXIS2_PLACEMENT_3D ( 'NONE', #402, #1398, #2198 ) ;
#9805 = EDGE_CURVE ( 'NONE', #10254, #8117, #9925, .T. ) ;
#9806 = EDGE_LOOP ( 'NONE', ( #3212, #12281, #1290, #7859 ) ) ;
#9807 = AXIS2_PLACEMENT_3D ( 'NONE', #854, #10683, #4859 ) ;
#9808 = CARTESIAN_POINT ( 'NONE',  ( 35.00000000000000000, 90.00000000000000000, 4.000000000000000000 ) ) ;
#9809 = VERTEX_POINT ( 'NONE', #7906 ) ;
#9810 = DIRECTION ( 'NONE',  ( -1.000000000000000000, -0.000000000000000000, -0.000000000000000000 ) ) ;
#9811 = LINE ( 'NONE', #5878, #8328 ) ;
#9812 = VECTOR ( 'NONE', #1117, 1000.000000000000000 ) ;
#9813 = ORIENTED_EDGE ( 'NONE', *, *, #4154, .F. ) ;
#9814 = SPHERICAL_SURFACE ( 'NONE', #1996, 3.351416843938787249 ) ;
#9815 = EDGE_LOOP ( 'NONE', ( #5633, #8652, #12284, #1386 ) ) ;
#9816 = DIRECTION ( 'NONE',  ( -1.000000000000000000, -0.000000000000000000, -0.000000000000000000 ) ) ;
#9817 = EDGE_CURVE ( 'NONE', #10905, #10264, #10717, .T. ) ;
#9818 = ORIENTED_EDGE ( 'NONE', *, *, #9680, .T. ) ;
#9819 = CARTESIAN_POINT ( 'NONE',  ( 35.00000000000000711, 53.69209320379640360, 3.115625000614517415 ) ) ;
#9820 = ORIENTED_EDGE ( 'NONE', *, *, #10364, .F. ) ;
#9821 = CIRCLE ( 'NONE', #6049, 4.338286831716297698 ) ;
#9822 = CARTESIAN_POINT ( 'NONE',  ( 2.168404344971008868E-16, -0.5773502691896253980, 1.000000000000000000 ) ) ;
#9823 = CARTESIAN_POINT ( 'NONE',  ( 8.499999999999998224, 69.54849343948981755, 1.000000000000000000 ) ) ;
#9824 = DIRECTION ( 'NONE',  ( -0.000000000000000000, -1.000000000000000000, -0.000000000000000000 ) ) ;
#9825 = CARTESIAN_POINT ( 'NONE',  ( 3.556430356250028790, 71.84604660189818048, 3.490625000614517415 ) ) ;
#9826 = ADVANCED_FACE ( 'NONE', ( #11764 ), #11892, .T. ) ;
#9827 = DIRECTION ( 'NONE',  ( -1.000000000000000000, -0.000000000000000000, -0.000000000000000000 ) ) ;
#9828 = CARTESIAN_POINT ( 'NONE',  ( 50.60000000000001563, 62.98000740192552627, 4.700000000000000178 ) ) ;
#9829 = CARTESIAN_POINT ( 'NONE',  ( 35.00000000000000000, 90.00000000000000000, 4.000000000000000000 ) ) ;
#9830 = CARTESIAN_POINT ( 'NONE',  ( 35.00000000000000000, 90.00000000000000000, 4.000000000000000000 ) ) ;
#9831 = DIRECTION ( 'NONE',  ( -0.000000000000000000, -1.000000000000000000, -0.000000000000000000 ) ) ;
#9832 = EDGE_CURVE ( 'NONE', #9660, #4244, #11701, .T. ) ;
#9833 = DIRECTION ( 'NONE',  ( 0.4719909656437442647, -0.8816033849473842166, 2.775557561595757269E-17 ) ) ;
#9834 = ORIENTED_EDGE ( 'NONE', *, *, #11090, .T. ) ;
#9835 = CARTESIAN_POINT ( 'NONE',  ( 34.25000000000000000, 93.50000000000000000, -3.000000000000000000 ) ) ;
#9836 = CARTESIAN_POINT ( 'NONE',  ( 35.00000000000000000, 126.3079067962035822, 4.746875000614517504 ) ) ;
#9837 = ORIENTED_EDGE ( 'NONE', *, *, #7034, .T. ) ;
#9838 = CARTESIAN_POINT ( 'NONE',  ( 35.00000000000000000, 126.0266567974326222, 3.537500000000000089 ) ) ;
#9839 = AXIS2_PLACEMENT_3D ( 'NONE', #7943, #4866, #8853 ) ;
#9840 = CARTESIAN_POINT ( 'NONE',  ( 3.800000000000015365, 90.00000000000000000, 3.762500001229034385 ) ) ;
#9841 = ORIENTED_EDGE ( 'NONE', *, *, #7399, .F. ) ;
#9842 = EDGE_CURVE ( 'NONE', #3791, #11492, #6660, .T. ) ;
#9843 = DIRECTION ( 'NONE',  ( 0.000000000000000000, 0.000000000000000000, 1.000000000000000000 ) ) ;
#9844 = CARTESIAN_POINT ( 'NONE',  ( 7.264852530253062213, 98.48596457872582732, 0.6666666666666654084 ) ) ;
#9845 = VECTOR ( 'NONE', #3290, 1000.000000000000000 ) ;
#9846 = CARTESIAN_POINT ( 'NONE',  ( 35.00000000000000000, 90.00000000000000000, 6.000000000000000000 ) ) ;
#9847 = CARTESIAN_POINT ( 'NONE',  ( 50.72178482187499071, 117.2309300971526937, 2.853125000614517237 ) ) ;
#9848 = CARTESIAN_POINT ( 'NONE',  ( -18.33333333333332504, 2.000000000000000000, 7.999999999999996447 ) ) ;
#9849 = CARTESIAN_POINT ( 'NONE',  ( 19.27821517812503060, 62.76906990284727783, 4.484375000614516438 ) ) ;
#9850 = ORIENTED_EDGE ( 'NONE', *, *, #5381, .T. ) ;
#9851 = SPHERICAL_SURFACE ( 'NONE', #3081, 3.351416843938785028 ) ;
#9852 = EDGE_LOOP ( 'NONE', ( #968, #3464, #9877 ) ) ;
#9853 = CARTESIAN_POINT ( 'NONE',  ( -53.07079676972452376, 33.99826794919245998, 1.000000000000000000 ) ) ;
#9854 = PRODUCT_DEFINITION ( 'UNKNOWN', '', #6129, #10393 ) ;
#9855 = DIRECTION ( 'NONE',  ( 0.000000000000000000, 0.000000000000000000, -1.000000000000000000 ) ) ;
#9856 = CARTESIAN_POINT ( 'NONE',  ( 3.556430356250015024, 90.00000000000000000, 4.859375000614517326 ) ) ;
#9857 = EDGE_CURVE ( 'NONE', #3989, #6259, #6917, .T. ) ;
#9858 = LINE ( 'NONE', #886, #11361 ) ;
#9859 = CARTESIAN_POINT ( 'NONE',  ( 4.270088556250601699E-16, 30.00000000000000000, -8.000000000000000000 ) ) ;
#9860 = ORIENTED_EDGE ( 'NONE', *, *, #1029, .F. ) ;
#9861 = PLANE ( 'NONE',  #8054 ) ;
#9862 = LINE ( 'NONE', #890, #8572 ) ;
#9863 = EDGE_LOOP ( 'NONE', ( #1234, #9450, #1150, #11321 ) ) ;
#9864 = CIRCLE ( 'NONE', #2348, 1.599999999999998090 ) ;
#9865 = CARTESIAN_POINT ( 'NONE',  ( 1.040000000000000036, -0.5773502691896253980, -1.000000000000000000 ) ) ;
#9866 = VERTEX_POINT ( 'NONE', #5811 ) ;
#9867 = ORIENTED_EDGE ( 'NONE', *, *, #6025, .T. ) ;
#9868 = CARTESIAN_POINT ( 'NONE',  ( 3.800000000000055334, 71.98667160128364628, 4.137500000000000178 ) ) ;
#9869 = CARTESIAN_POINT ( 'NONE',  ( 50.00000000000000000, 62.64236852357281293, -1.499999999999999778 ) ) ;
#9870 = EDGE_CURVE ( 'NONE', #11286, #2819, #9192, .T. ) ;
#9871 = CONICAL_SURFACE ( 'NONE', #5059, 1.500000000000001332, 1.029744260000000411 ) ;
#9872 = ADVANCED_FACE ( 'NONE', ( #10904 ), #5746, .T. ) ;
#9873 = EDGE_LOOP ( 'NONE', ( #8322, #6978, #4444, #4832 ) ) ;
#9874 = DIRECTION ( 'NONE',  ( -0.000000000000000000, -0.5000000000000000000, 0.8660254037844385966 ) ) ;
#9875 = ORIENTED_EDGE ( 'NONE', *, *, #7411, .T. ) ;
#9876 = DIRECTION ( 'NONE',  ( 1.000000000000000000, 0.000000000000000000, 0.000000000000000000 ) ) ;
#9877 = ORIENTED_EDGE ( 'NONE', *, *, #3048, .T. ) ;
#9878 = CARTESIAN_POINT ( 'NONE',  ( 50.72178482187501203, 62.76906990284730625, 3.603125000614517681 ) ) ;
#9879 = EDGE_LOOP ( 'NONE', ( #9960, #9277, #11561, #10544 ) ) ;
#9880 = VECTOR ( 'NONE', #6971, 1000.000000000000000 ) ;
#9881 = DIRECTION ( 'NONE',  ( 0.000000000000000000, 0.000000000000000000, 1.000000000000000000 ) ) ;
#9882 = DIRECTION ( 'NONE',  ( -0.000000000000000000, -0.000000000000000000, -1.000000000000000000 ) ) ;
#9883 = LINE ( 'NONE', #3946, #669 ) ;
#9884 = CARTESIAN_POINT ( 'NONE',  ( 66.20000000000000284, 71.98667160128370313, 4.400000001229034119 ) ) ;
#9885 = VECTOR ( 'NONE', #1777, 1000.000000000000000 ) ;
#9886 = ADVANCED_FACE ( 'NONE', ( #2812 ), #12752, .T. ) ;
#9887 = DIRECTION ( 'NONE',  ( 0.000000000000000000, 0.000000000000000000, 1.000000000000000000 ) ) ;
#9888 = ORIENTED_EDGE ( 'NONE', *, *, #188, .F. ) ;
#9889 = CARTESIAN_POINT ( 'NONE',  ( 35.00000000000000000, 90.00000000000000000, -10.00000000000000000 ) ) ;
#9890 = CARTESIAN_POINT ( 'NONE',  ( 1.599999999999999867, -4.873461295629625489, 0.000000000000000000 ) ) ;
#9891 = CARTESIAN_POINT ( 'NONE',  ( 15.50185732988873077, 114.6638150138266639, 2.999999999999999112 ) ) ;
#9892 = VERTEX_POINT ( 'NONE', #12689 ) ;
#9893 = AXIS2_PLACEMENT_3D ( 'NONE', #6056, #3789, #7768 ) ;
#9894 = CARTESIAN_POINT ( 'NONE',  ( 52.49999999999996447, 86.00000000000000000, -10.00000000000000000 ) ) ;
#9895 = VERTEX_POINT ( 'NONE', #4834 ) ;
#9896 = DIRECTION ( 'NONE',  ( 1.914177628664063178E-15, -1.000000000000000000, 0.000000000000000000 ) ) ;
#9897 = CARTESIAN_POINT ( 'NONE',  ( 3.556430356250014579, 108.1539533981018053, 4.371875000614517504 ) ) ;
#9898 = ORIENTED_EDGE ( 'NONE', *, *, #5548, .T. ) ;
#9899 = ORIENTED_EDGE ( 'NONE', *, *, #4794, .T. ) ;
#9900 = CARTESIAN_POINT ( 'NONE',  ( 3.556430356250014579, 108.1539533981018053, 4.821875000614516793 ) ) ;
#9901 = FACE_OUTER_BOUND ( 'NONE', #6992, .T. ) ;
#9902 = EDGE_CURVE ( 'NONE', #6195, #8482, #7311, .T. ) ;
#9903 = CIRCLE ( 'NONE', #6979, 30.00000000000000000 ) ;
#9904 = PRESENTATION_LAYER_ASSIGNMENT (  '', '', ( #9491 ) ) ;
#9905 = FILL_AREA_STYLE_COLOUR ( '', #9063 ) ;
#9906 = CARTESIAN_POINT ( 'NONE',  ( -31.49999999999998579, 79.07477288111861924, -1.000000000000000000 ) ) ;
#9907 = CLOSED_SHELL ( 'NONE', ( #6918, #10626, #4390, #11722, #3362, #1943, #8199, #11883, #11261, #1850, #9039, #10149, #5513, #5992, #1322, #12473, #2201, #6240, #141, #5296, #3041, #10794, #223, #6559, #10272, #12827, #1458, #7488, #873, #7559 ) ) ;
#9908 = DIRECTION ( 'NONE',  ( 0.8090169943749456749, -0.5877852522924754686, 0.000000000000000000 ) ) ;
#9909 = EDGE_CURVE ( 'NONE', #3811, #2543, #3731, .T. ) ;
#9910 = EDGE_CURVE ( 'NONE', #1278, #1585, #7649, .T. ) ;
#9911 = LINE ( 'NONE', #942, #10034 ) ;
#9912 = VECTOR ( 'NONE', #737, 1000.000000000000000 ) ;
#9913 = FACE_OUTER_BOUND ( 'NONE', #11095, .T. ) ;
#9914 = ORIENTED_EDGE ( 'NONE', *, *, #11632, .F. ) ;
#9915 = DIRECTION ( 'NONE',  ( 1.000000000000000000, 0.000000000000000000, 5.337610695313252124E-17 ) ) ;
#9916 = ORIENTED_EDGE ( 'NONE', *, *, #7789, .T. ) ;
#9917 = CARTESIAN_POINT ( 'NONE',  ( 38.50000000000000711, 90.00000000000000000, -3.000000000000000888 ) ) ;
#9918 = DIRECTION ( 'NONE',  ( -1.000000000000000000, 0.000000000000000000, 0.000000000000000000 ) ) ;
#9919 = VECTOR ( 'NONE', #6641, 1000.000000000000114 ) ;
#9920 = DIRECTION ( 'NONE',  ( -0.8660254037844393737, -0.4999999999999987232, 0.000000000000000000 ) ) ;
#9921 = VECTOR ( 'NONE', #2031, 1000.000000000000000 ) ;
#9922 = ORIENTED_EDGE ( 'NONE', *, *, #12440, .F. ) ;
#9923 = FACE_OUTER_BOUND ( 'NONE', #9325, .T. ) ;
#9924 = CONTEXT_DEPENDENT_SHAPE_REPRESENTATION ( #6264, #7004 ) ;
#9925 = LINE ( 'NONE', #11831, #11065 ) ;
#9926 = VERTEX_POINT ( 'NONE', #7772 ) ;
#9927 = PRODUCT_RELATED_PRODUCT_CATEGORY ( 'part', '', ( #8352 ) ) ;
#9928 =( NAMED_UNIT ( * ) PLANE_ANGLE_UNIT ( ) SI_UNIT ( $, .RADIAN. ) );
#9929 = DIRECTION ( 'NONE',  ( 0.000000000000000000, 0.000000000000000000, -1.000000000000000000 ) ) ;
#9930 = VERTEX_POINT ( 'NONE', #7713 ) ;
#9931 = FACE_OUTER_BOUND ( 'NONE', #1925, .T. ) ;
#9933 = EDGE_LOOP ( 'NONE', ( #4187, #3075, #10584, #9899 ) ) ;
#9932 = VECTOR ( 'NONE', #3315, 1000.000000000000000 ) ;
#9934 = EDGE_CURVE ( 'NONE', #9892, #11514, #1883, .T. ) ;
#9935 = CIRCLE ( 'NONE', #4924, 1.000000000000000000 ) ;
#9936 = DIRECTION ( 'NONE',  ( -0.9549484348006339607, -0.2967717757331703732, 0.000000000000000000 ) ) ;
#9937 = SHAPE_REPRESENTATION ( 'sorter block', ( #5704 ), #258 ) ;
#9938 = DIRECTION ( 'NONE',  ( -0.000000000000000000, 1.000000000000000000, -0.000000000000000000 ) ) ;
#9939 = VERTEX_POINT ( 'NONE', #8818 ) ;
#9940 = EDGE_LOOP ( 'NONE', ( #4189, #771 ) ) ;
#9941 = CARTESIAN_POINT ( 'NONE',  ( 30.00000000000000711, 2.000000000000000000, -1.499999999999999556 ) ) ;
#9942 = ORIENTED_EDGE ( 'NONE', *, *, #1200, .F. ) ;
#9943 = VECTOR ( 'NONE', #11862, 1000.000000000000000 ) ;
#9944 = DIRECTION ( 'NONE',  ( -1.000000000000000000, -0.000000000000000000, -0.000000000000000000 ) ) ;
#9945 = EDGE_LOOP ( 'NONE', ( #4015, #5765, #10671, #7941, #4109, #7651, #12570, #11122, #1256, #9619, #7256, #4372 ) ) ;
#9946 = EDGE_CURVE ( 'NONE', #1140, #5809, #9821, .T. ) ;
#9947 = CARTESIAN_POINT ( 'NONE',  ( 35.00000000000000000, 126.3079067962035822, 4.240625000614517859 ) ) ;
#9948 = ORIENTED_EDGE ( 'NONE', *, *, #8474, .T. ) ;
#9949 = CARTESIAN_POINT ( 'NONE',  ( -6.666666666666660745, 2.000000000000000000, 0.000000000000000000 ) ) ;
#9950 = CARTESIAN_POINT ( 'NONE',  ( 60.00000000000000000, 0.000000000000000000, 15.00000000000000000 ) ) ;
#9951 = EDGE_CURVE ( 'NONE', #193, #10175, #9862, .T. ) ;
#9952 = CARTESIAN_POINT ( 'NONE',  ( 66.20000000000005969, 108.0133283987162685, 4.812499999999999112 ) ) ;
#9953 = CARTESIAN_POINT ( 'NONE',  ( 66.19999999999998863, 90.00000000000000000, 3.987500001229034030 ) ) ;
#9954 = CIRCLE ( 'NONE', #9121, 1.599999999999986766 ) ;
#9955 = PLANE ( 'NONE',  #11269 ) ;
#9956 = ORIENTED_EDGE ( 'NONE', *, *, #12108, .F. ) ;
#9957 = LINE ( 'NONE', #4861, #12648 ) ;
#9958 = DIRECTION ( 'NONE',  ( 0.000000000000000000, 0.000000000000000000, -1.000000000000000000 ) ) ;
#9959 = CARTESIAN_POINT ( 'NONE',  ( 0.000000000000000000, 1.836970198721028208E-16, -1.499999999999998668 ) ) ;
#9960 = ORIENTED_EDGE ( 'NONE', *, *, #1029, .T. ) ;
#9961 = DIRECTION ( 'NONE',  ( -1.000000000000000000, 0.000000000000000000, 0.000000000000000000 ) ) ;
#9962 = ORIENTED_EDGE ( 'NONE', *, *, #12932, .F. ) ;
#9963 = EDGE_CURVE ( 'NONE', #5827, #6538, #2684, .T. ) ;
#9964 = CIRCLE ( 'NONE', #5986, 1.500000000000003331 ) ;
#9965 = CARTESIAN_POINT ( 'NONE',  ( 3.800000000000015365, 90.00000000000000000, 5.000000000000000000 ) ) ;
#9966 = CARTESIAN_POINT ( 'NONE',  ( 3.556430356250028790, 71.84604660189818048, 3.040625000614517237 ) ) ;
#9967 = ORIENTED_EDGE ( 'NONE', *, *, #2336, .T. ) ;
#9968 = CARTESIAN_POINT ( 'NONE',  ( 3.556430356250014579, 108.1539533981018053, 3.021875000614517415 ) ) ;
#9969 = CARTESIAN_POINT ( 'NONE',  ( 66.20000000000004547, 108.0133283987162969, 3.575000001229034385 ) ) ;
#9970 = AXIS2_PLACEMENT_3D ( 'NONE', #5785, #12727, #6958 ) ;
#9971 = FACE_OUTER_BOUND ( 'NONE', #6983, .T. ) ;
#9972 = DIRECTION ( 'NONE',  ( -0.000000000000000000, 0.000000000000000000, -1.000000000000000000 ) ) ;
#9973 = CARTESIAN_POINT ( 'NONE',  ( 45.00000000000000000, 0.000000000000000000, -5.750000000000000000 ) ) ;
#9974 = EDGE_CURVE ( 'NONE', #3079, #1986, #8943, .T. ) ;
#9975 = PLANE ( 'NONE',  #8785 ) ;
#9976 = CARTESIAN_POINT ( 'NONE',  ( 35.00000000000000000, 90.00000000000000000, 5.000000000000000000 ) ) ;
#9977 = ORIENTED_EDGE ( 'NONE', *, *, #4163, .T. ) ;
#9978 = VECTOR ( 'NONE', #187, 1000.000000000000000 ) ;
#9979 = CARTESIAN_POINT ( 'NONE',  ( 40.00000000000000000, 0.000000000000000000, 10.00000000000000000 ) ) ;
#9980 = ORIENTED_EDGE ( 'NONE', *, *, #10170, .F. ) ;
#9981 = CARTESIAN_POINT ( 'NONE',  ( 33.50000000000000711, 79.80000000000001137, 6.000000000000000000 ) ) ;
#9982 = EDGE_CURVE ( 'NONE', #7180, #3927, #1461, .T. ) ;
#9983 = EDGE_CURVE ( 'NONE', #7103, #1898, #4243, .T. ) ;
#9984 = DIRECTION ( 'NONE',  ( 0.000000000000000000, 0.000000000000000000, 1.000000000000000000 ) ) ;
#9985 = DIRECTION ( 'NONE',  ( -0.000000000000000000, 1.000000000000000000, -0.000000000000000000 ) ) ;
#9986 = AXIS2_PLACEMENT_3D ( 'NONE', #8028, #2805, #9855 ) ;
#9987 = CARTESIAN_POINT ( 'NONE',  ( -1.625004804578467077, -6.241943558307533557, 0.000000000000000000 ) ) ;
#9988 = AXIS2_PLACEMENT_3D ( 'NONE', #7721, #11900, #777 ) ;
#9989 = ORIENTED_EDGE ( 'NONE', *, *, #3757, .F. ) ;
#9990 = DIRECTION ( 'NONE',  ( 0.000000000000000000, -1.000000000000000000, 0.000000000000000000 ) ) ;
#9991 = ITEM_DEFINED_TRANSFORMATION ( 'NONE', 'NONE', #8857,  #5704 ) ;
#9992 = DIRECTION ( 'NONE',  ( 0.000000000000000000, 0.000000000000000000, 1.000000000000000000 ) ) ;
#9993 = VERTEX_POINT ( 'NONE', #7175 ) ;
#9994 = EDGE_CURVE ( 'NONE', #12910, #7130, #8185, .T. ) ;
#9995 = FACE_OUTER_BOUND ( 'NONE', #9349, .T. ) ;
#9996 = VERTEX_POINT ( 'NONE', #1286 ) ;
#9997 = CARTESIAN_POINT ( 'NONE',  ( -61.00000000000000711, 26.13129029178200469, -0.9999999999999931166 ) ) ;
#9998 = ORIENTED_EDGE ( 'NONE', *, *, #4406, .T. ) ;
#9999 = AXIS2_PLACEMENT_3D ( 'NONE', #2801, #762, #12743 ) ;
#10000 = FACE_OUTER_BOUND ( 'NONE', #1499, .T. ) ;
#10001 = DIRECTION ( 'NONE',  ( -0.000000000000000000, 1.000000000000000000, -0.000000000000000000 ) ) ;
#10002 = ORIENTED_EDGE ( 'NONE', *, *, #7198, .F. ) ;
#10003 = EDGE_LOOP ( 'NONE', ( #1889, #5985, #4064, #10058, #3344, #12295 ) ) ;
#10004 = CARTESIAN_POINT ( 'NONE',  ( 36.58116973490655255, 87.04662866042625069, -3.799999999999999822 ) ) ;
#10005 = VERTEX_POINT ( 'NONE', #3269 ) ;
#10006 = EDGE_CURVE ( 'NONE', #3338, #6015, #2927, .T. ) ;
#10007 = CARTESIAN_POINT ( 'NONE',  ( 3.556430356250028790, 71.84604660189818048, 3.490625000614517415 ) ) ;
#10008 = CIRCLE ( 'NONE', #7295, 1.499999999999998668 ) ;
#10009 = ORIENTED_EDGE ( 'NONE', *, *, #4300, .F. ) ;
#10010 = CARTESIAN_POINT ( 'NONE',  ( 3.800000000000025580, 71.98667160128366049, 3.350000001229034297 ) ) ;
#10011 = VERTEX_POINT ( 'NONE', #8227 ) ;
#10012 =( BOUNDED_CURVE ( )  B_SPLINE_CURVE ( 2, ( #8060, #12901, #3158, #6019, #52, #9952, #8840 ),
 .UNSPECIFIED., .F., .F. ) 
 B_SPLINE_CURVE_WITH_KNOTS ( ( 3, 2, 2, 3 ),
 ( 0.000000000000000000, 0.03333333333333339532, 0.06666666666666679064, 0.1000000000000001860 ),
 .UNSPECIFIED. ) 
 CURVE ( )  GEOMETRIC_REPRESENTATION_ITEM ( )  RATIONAL_B_SPLINE_CURVE ( ( 1.000000000000000000, 0.8660254037844387076, 1.000000000000000000, 0.8660254037844387076, 1.000000000000000000, 0.8660254037844380415, 1.000000000000000666 ) ) 
 REPRESENTATION_ITEM ( '' )  );
#10013 = LINE ( 'NONE', #7792, #4838 ) ;
#10014 = CARTESIAN_POINT ( 'NONE',  ( 3.556430356250015024, 90.00000000000000000, 4.353125000614517681 ) ) ;
#10015 = AXIS2_PLACEMENT_3D ( 'NONE', #7728, #4724, #6933 ) ;
#10016 = CARTESIAN_POINT ( 'NONE',  ( 19.40000000000000924, 117.0199925980744666, 3.237500001229034030 ) ) ;
#10017 =( LENGTH_UNIT ( ) NAMED_UNIT ( * ) SI_UNIT ( .MILLI., .METRE. ) );
#10018 = PLANE ( 'NONE',  #177 ) ;
#10019 = ORIENTED_EDGE ( 'NONE', *, *, #5002, .F. ) ;
#10020 = CARTESIAN_POINT ( 'NONE',  ( 60.43447242791587826, 111.3420572944792895, 3.026359441279048657 ) ) ;
#10021 = EDGE_CURVE ( 'NONE', #9204, #1482, #159, .T. ) ;
#10022 = FACE_OUTER_BOUND ( 'NONE', #2152, .T. ) ;
#10023 = CARTESIAN_POINT ( 'NONE',  ( 62.18023010225326175, 105.5722019109657310, 2.999999999999999556 ) ) ;
#10024 = ORIENTED_EDGE ( 'NONE', *, *, #48, .T. ) ;
#10025 = VECTOR ( 'NONE', #1697, 1000.000000000000000 ) ;
#10026 = CARTESIAN_POINT ( 'NONE',  ( 1.040000000000000036, -1.154700538379251684, 0.000000000000000000 ) ) ;
#10027 = ORIENTED_EDGE ( 'NONE', *, *, #11102, .F. ) ;
#10028 = DIRECTION ( 'NONE',  ( 0.5877852522924726930, -0.8090169943749476733, -0.000000000000000000 ) ) ;
#10029 = CARTESIAN_POINT ( 'NONE',  ( 66.44356964374999563, 71.84604660189820891, 3.190625000614517592 ) ) ;
#10030 = EDGE_LOOP ( 'NONE', ( #4482, #11686, #10200, #434, #1759, #5502 ) ) ;
#10031 = CARTESIAN_POINT ( 'NONE',  ( 50.72178482187499071, 117.2309300971526937, 4.709375000614516971 ) ) ;
#10032 = DIRECTION ( 'NONE',  ( 0.000000000000000000, 0.000000000000000000, 1.000000000000000000 ) ) ;
#10033 = CARTESIAN_POINT ( 'NONE',  ( 1.040000000000000036, 0.5773502691896263972, -1.000000000000000000 ) ) ;
#10034 = VECTOR ( 'NONE', #8929, 1000.000000000000000 ) ;
#10035 = ADVANCED_FACE ( 'NONE', ( #3133, #5277 ), #2284, .F. ) ;
#10036 = DIRECTION ( 'NONE',  ( 0.000000000000000000, -1.000000000000000000, 0.000000000000000000 ) ) ;
#10037 = EDGE_CURVE ( 'NONE', #451, #6711, #11228, .T. ) ;
#10038 = CARTESIAN_POINT ( 'NONE',  ( 0.000000000000000000, 0.4117131682837005258, -0.8000000000000000444 ) ) ;
#10039 = DIRECTION ( 'NONE',  ( 0.000000000000000000, 0.000000000000000000, 1.000000000000000000 ) ) ;
#10040 = AXIS2_PLACEMENT_3D ( 'NONE', #2973, #8072, #8919 ) ;
#10041 = DIRECTION ( 'NONE',  ( 0.000000000000000000, 0.000000000000000000, 1.000000000000000000 ) ) ;
#10042 = CARTESIAN_POINT ( 'NONE',  ( 66.44356964374999563, 90.00000000000000000, 3.284375000614517148 ) ) ;
#10043 = EDGE_LOOP ( 'NONE', ( #8522, #7236, #2809, #11716 ) ) ;
#10044 = CARTESIAN_POINT ( 'NONE',  ( 62.42613047537196991, 99.43702109502110886, 2.333333333333333481 ) ) ;
#10045 = EDGE_LOOP ( 'NONE', ( #12694, #12164, #2965, #7364 ) ) ;
#10046 = EDGE_CURVE ( 'NONE', #2484, #10256, #3198, .T. ) ;
#10047 = DIRECTION ( 'NONE',  ( -0.8660254037844397068, -0.4999999999999985567, -0.000000000000000000 ) ) ;
#10048 = DIRECTION ( 'NONE',  ( 1.000000000000000000, 0.000000000000000000, 0.000000000000000000 ) ) ;
#10049 = DIRECTION ( 'NONE',  ( 1.000000000000000000, 0.000000000000000000, 2.891205793294678696E-17 ) ) ;
#10050 = VERTEX_POINT ( 'NONE', #7113 ) ;
#10051 = CARTESIAN_POINT ( 'NONE',  ( -48.33333333333332860, 2.000000000000001332, 1.599999999999988542 ) ) ;
#10052 = CARTESIAN_POINT ( 'NONE',  ( 3.800000000000025580, 71.98667160128366049, 3.687500000000000888 ) ) ;
#10053 = ORIENTED_EDGE ( 'NONE', *, *, #12275, .F. ) ;
#10054 = CARTESIAN_POINT ( 'NONE',  ( 30.00000000000000711, 90.00000000000000000, -8.000000000000000000 ) ) ;
#10055 = ORIENTED_EDGE ( 'NONE', *, *, #10889, .T. ) ;
#10056 =( GEOMETRIC_REPRESENTATION_CONTEXT ( 3 ) GLOBAL_UNCERTAINTY_ASSIGNED_CONTEXT ( ( #3326 ) ) GLOBAL_UNIT_ASSIGNED_CONTEXT ( ( #11835, #10850, #3928 ) ) REPRESENTATION_CONTEXT ( 'NONE', 'WORKASPACE' ) );
#10057 = FILL_AREA_STYLE ('',( #10190 ) ) ;
#10058 = ORIENTED_EDGE ( 'NONE', *, *, #6879, .T. ) ;
#10059 = CARTESIAN_POINT ( 'NONE',  ( 36.58116973490655255, 87.04662866042625069, -3.000000000000000000 ) ) ;
#10060 = DIRECTION ( 'NONE',  ( 0.000000000000000000, 0.000000000000000000, 1.000000000000000000 ) ) ;
#10061 = ORIENTED_EDGE ( 'NONE', *, *, #8865, .T. ) ;
#10062 = ORIENTED_EDGE ( 'NONE', *, *, #2481, .T. ) ;
#10063 = DIRECTION ( 'NONE',  ( 0.000000000000000000, 0.000000000000000000, 1.000000000000000000 ) ) ;
#10064 = EDGE_LOOP ( 'NONE', ( #181, #3147, #3008, #12027 ) ) ;
#10065 = PRODUCT_CONTEXT ( 'NONE', #6833, 'mechanical' ) ;
#10066 = CARTESIAN_POINT ( 'NONE',  ( 3.556430356250014579, 108.1539533981018053, 2.965625000614517504 ) ) ;
#10067 = ORIENTED_EDGE ( 'NONE', *, *, #4050, .T. ) ;
#10068 = FACE_BOUND ( 'NONE', #6722, .T. ) ;
#10069 = EDGE_CURVE ( 'NONE', #12641, #12892, #5995, .T. ) ;
#10070 = ORIENTED_EDGE ( 'NONE', *, *, #4651, .T. ) ;
#10071 = EDGE_CURVE ( 'NONE', #2177, #4130, #11094, .T. ) ;
#10072 = CARTESIAN_POINT ( 'NONE',  ( 62.73102604205943322, 98.48470356904833523, 2.000000000000001776 ) ) ;
#10073 = CYLINDRICAL_SURFACE ( 'NONE', #3293, 0.5999999999999999778 ) ;
#10074 = DIRECTION ( 'NONE',  ( -0.7071067811865489050, 0.000000000000000000, 0.7071067811865462405 ) ) ;
#10075 = CIRCLE ( 'NONE', #9454, 6.450000000000001066 ) ;
#10076 = DIRECTION ( 'NONE',  ( 1.000000000000000000, 0.000000000000000000, 0.000000000000000000 ) ) ;
#10077 = CARTESIAN_POINT ( 'NONE',  ( -60.00000000000000000, 30.00000000000000000, -8.000000000000003553 ) ) ;
#10078 = ORIENTED_EDGE ( 'NONE', *, *, #10426, .T. ) ;
#10079 = CARTESIAN_POINT ( 'NONE',  ( 50.72178482187501203, 62.76906990284730625, 4.559375000614517504 ) ) ;
#10080 = FACE_BOUND ( 'NONE', #118, .T. ) ;
#10081 = CARTESIAN_POINT ( 'NONE',  ( 1.749999999999999112, 1.836970198721028208E-16, -1.499999999999998668 ) ) ;
#10082 = ORIENTED_EDGE ( 'NONE', *, *, #516, .F. ) ;
#10083 =( BOUNDED_SURFACE ( )  B_SPLINE_SURFACE ( 1, 2, ( 
 ( #4784, #4321, #2301, #11045, #5163, #10202, #9087, #1038, #44, #8178, #12099, #2100, #6010, #10981, #4061, #7129, #8312, #5095, #9152, #114, #311, #6211, #2235, #5230, #10132, #7063, #12038, #1238, #176, #9217, #12298, #3284, #241, #7194, #11246, #10007, #1302, #5033, #4129, #8052, #9023, #8246, #6078, #3085, #4259, #7261, #2162, #6276, #3349, #10066, #1102, #12235, #10265, #5294, #8116 ),
 ( #3149, #9288, #11111, #4193, #6137, #2033, #1170, #12168, #3216, #11180, #11374, #10529, #2427, #8576, #5356, #11506, #11573, #374, #3604, #1566, #2620, #8507, #641, #1633, #6402, #439, #5554, #7524, #12363, #3410, #9352, #11309, #10597, #2554, #12627, #6533, #6597, #6468, #5621, #7325, #10400, #4645, #8634, #8379, #10464, #2492, #2360, #7585, #1432, #5420, #9613, #6335, #8440, #12564, #10335 ) ),
 .UNSPECIFIED., .F., .F., .F. ) 
 B_SPLINE_SURFACE_WITH_KNOTS ( ( 2, 2 ),
 ( 3, 2, 2, 2, 2, 2, 2, 2, 2, 2, 2, 2, 2, 2, 2, 2, 2, 2, 2, 2, 2, 2, 2, 2, 2, 2, 2, 3 ),
 ( 0.000000000000000000, 1.000000000000000000 ),
 ( 0.000000000000000000, 0.03333333333333333287, 0.06666666666666666574, 0.1000000000000000056, 0.1333333333333333315, 0.1666666666666666574, 0.2000000000000000111, 0.2333333333333333370, 0.2666666666666666630, 0.2999999999999999889, 0.3333333333333333148, 0.3666666666666666408, 0.4000000000000000222, 0.4333333333333333481, 0.4666666666666666741, 0.5000000000000000000, 0.5333333333333333259, 0.5666666666666666519, 0.5999999999999999778, 0.6333333333333333037, 0.6666666666666666297, 0.6999999999999999556, 0.7333333333333332815, 0.7666666666666667185, 0.8000000000000000444, 0.8333333333333333703, 0.8666666666666666963, 0.8887752010635167066 ),
 .UNSPECIFIED. ) 
 GEOMETRIC_REPRESENTATION_ITEM ( )  RATIONAL_B_SPLINE_SURFACE ( (
 ( 1.000000000000000000, 0.8660254037844387076, 1.000000000000000000, 0.8660254037844387076, 1.000000000000000000, 0.8660254037844387076, 1.000000000000000000, 0.8660254037844387076, 1.000000000000000000, 0.8660254037844387076, 1.000000000000000000, 0.8660254037844387076, 1.000000000000000000, 0.8660254037844387076, 1.000000000000000000, 0.8660254037844387076, 1.000000000000000000, 0.8660254037844387076, 1.000000000000000000, 0.8660254037844387076, 1.000000000000000000, 0.8660254037844387076, 1.000000000000000000, 0.8660254037844387076, 1.000000000000000000, 0.8660254037844387076, 1.000000000000000000, 0.8660254037844387076, 1.000000000000000000, 0.8660254037844387076, 1.000000000000000000, 0.8660254037844387076, 1.000000000000000000, 0.8660254037844387076, 1.000000000000000000, 0.8660254037844387076, 1.000000000000000000, 0.8660254037844387076, 1.000000000000000000, 0.8660254037844387076, 1.000000000000000000, 0.8660254037844387076, 1.000000000000000000, 0.8660254037844387076, 1.000000000000000000, 0.8660254037844387076, 1.000000000000000000, 0.8660254037844387076, 1.000000000000000000, 0.8660254037844387076, 1.000000000000000000, 0.8660254037844387076, 1.000000000000000000, 0.9111405409379251807, 0.9401542263054123438),
 ( 1.000000000000000000, 0.8660254037844387076, 1.000000000000000000, 0.8660254037844387076, 1.000000000000000000, 0.8660254037844387076, 1.000000000000000000, 0.8660254037844387076, 1.000000000000000000, 0.8660254037844387076, 1.000000000000000000, 0.8660254037844387076, 1.000000000000000000, 0.8660254037844387076, 1.000000000000000000, 0.8660254037844387076, 1.000000000000000000, 0.8660254037844387076, 1.000000000000000000, 0.8660254037844387076, 1.000000000000000000, 0.8660254037844387076, 1.000000000000000000, 0.8660254037844387076, 1.000000000000000000, 0.8660254037844387076, 1.000000000000000000, 0.8660254037844387076, 1.000000000000000000, 0.8660254037844387076, 1.000000000000000000, 0.8660254037844387076, 1.000000000000000000, 0.8660254037844387076, 1.000000000000000000, 0.8660254037844387076, 1.000000000000000000, 0.8660254037844387076, 1.000000000000000000, 0.8660254037844387076, 1.000000000000000000, 0.8660254037844387076, 1.000000000000000000, 0.8660254037844387076, 1.000000000000000000, 0.8660254037844387076, 1.000000000000000000, 0.8660254037844387076, 1.000000000000000000, 0.8660254037844387076, 1.000000000000000000, 0.8660254037844387076, 1.000000000000000000, 0.9111405409379251807, 0.9401542263054123438) ) ) 
 REPRESENTATION_ITEM ( '' )  SURFACE ( )  );
#10084 = DIRECTION ( 'NONE',  ( 0.000000000000000000, 0.000000000000000000, 1.000000000000000000 ) ) ;
#10085 = ORIENTED_EDGE ( 'NONE', *, *, #7925, .T. ) ;
#10086 = CARTESIAN_POINT ( 'NONE',  ( 18.35999867260799689, 66.24638416932324958, -1.000000000000000000 ) ) ;
#10087 = AXIS2_PLACEMENT_3D ( 'NONE', #885, #823, #4889 ) ;
#10088 = UNCERTAINTY_MEASURE_WITH_UNIT (LENGTH_MEASURE( 1.000000000000000082E-05 ), #1367, 'distance_accuracy_value', 'NONE');
#10089 = CARTESIAN_POINT ( 'NONE',  ( 19.27821517812503060, 62.76906990284727783, 3.528125000614517059 ) ) ;
#10090 = ORIENTED_EDGE ( 'NONE', *, *, #6103, .F. ) ;
#10091 = CARTESIAN_POINT ( 'NONE',  ( 35.00000000000000000, 126.3079067962035822, 3.846875000614517592 ) ) ;
#10092 = DIRECTION ( 'NONE',  ( -0.9510565162951529761, -0.3090169943749492276, 0.000000000000000000 ) ) ;
#10093 = EDGE_CURVE ( 'NONE', #6329, #5120, #6121, .T. ) ;
#10094 = DIRECTION ( 'NONE',  ( 0.000000000000000000, 0.000000000000000000, 1.000000000000000000 ) ) ;
#10095 = STYLED_ITEM ( 'NONE', ( #2150 ), #12938 ) ;
#10096 = DIRECTION ( 'NONE',  ( -0.000000000000000000, -0.000000000000000000, -1.000000000000000000 ) ) ;
#10097 = CLOSED_SHELL ( 'NONE', ( #855, #8466, #759, #5906, #633, #7705, #3275, #556, #4449, #3767, #6899, #1342, #2396, #2489, #6138, #8721, #6943, #471, #5605, #3817, #8526, #7896, #9886, #8996, #7071, #1802, #9559, #7319, #9708, #11218, #12033, #9519, #6622, #2756, #4107, #4397, #4623, #3095, #11302, #548, #10201, #4610, #8418, #3682, #7650, #8233, #4034, #8222, #5362, #2731, #5070, #6415, #2531, #8601, #11433 ) ) ;
#10098 = CARTESIAN_POINT ( 'NONE',  ( 35.00000000000000000, 90.00000000000000000, -8.000000000000000000 ) ) ;
#10099 = LINE ( 'NONE', #12135, #8449 ) ;
#10100 = CARTESIAN_POINT ( 'NONE',  ( 17.55170909815984004, 66.83416404266884570, 4.000000000000000000 ) ) ;
#10101 =( GEOMETRIC_REPRESENTATION_CONTEXT ( 3 ) GLOBAL_UNCERTAINTY_ASSIGNED_CONTEXT ( ( #10088 ) ) GLOBAL_UNIT_ASSIGNED_CONTEXT ( ( #1367, #5293, #9216 ) ) REPRESENTATION_CONTEXT ( 'NONE', 'WORKASPACE' ) );
#10102 = EDGE_CURVE ( 'NONE', #10917, #2666, #12548, .T. ) ;
#10103 = FACE_OUTER_BOUND ( 'NONE', #1166, .T. ) ;
#10104 = DIRECTION ( 'NONE',  ( -1.000000000000000000, -0.000000000000000000, -0.000000000000000000 ) ) ;
#10105 = ORIENTED_EDGE ( 'NONE', *, *, #11744, .T. ) ;
#10106 = CARTESIAN_POINT ( 'NONE',  ( 4.336808689942017736E-16, 1.424999999999999822, 0.000000000000000000 ) ) ;
#10107 = VERTEX_POINT ( 'NONE', #1221 ) ;
#10108 = AXIS2_PLACEMENT_3D ( 'NONE', #11143, #7291, #7160 ) ;
#10109 = EDGE_CURVE ( 'NONE', #12765, #6375, #827, .T. ) ;
#10110 = DIRECTION ( 'NONE',  ( -0.000000000000000000, 1.000000000000000000, 0.000000000000000000 ) ) ;
#10111 = DIRECTION ( 'NONE',  ( -0.000000000000000000, 1.000000000000000000, -0.000000000000000000 ) ) ;
#10112 = DIRECTION ( 'NONE',  ( 0.000000000000000000, 0.000000000000000000, 1.000000000000000000 ) ) ;
#10113 = VERTEX_POINT ( 'NONE', #9203 ) ;
#10114 = VECTOR ( 'NONE', #11667, 1000.000000000000000 ) ;
#10115 = DIRECTION ( 'NONE',  ( -0.000000000000000000, -0.000000000000000000, -1.000000000000000000 ) ) ;
#10116 = DIRECTION ( 'NONE',  ( -0.000000000000000000, -0.000000000000000000, 1.000000000000000000 ) ) ;
#10117 = AXIS2_PLACEMENT_3D ( 'NONE', #7611, #6947, #10744 ) ;
#10118 = VERTEX_POINT ( 'NONE', #28 ) ;
#10119 = ORIENTED_EDGE ( 'NONE', *, *, #9226, .F. ) ;
#10120 = EDGE_CURVE ( 'NONE', #12205, #6711, #6913, .T. ) ;
#10121 = CARTESIAN_POINT ( 'NONE',  ( -48.33333333333332860, 0.000000000000000000, -1.734723475976807094E-15 ) ) ;
#10122 = ORIENTED_EDGE ( 'NONE', *, *, #4912, .T. ) ;
#10123 = DIRECTION ( 'NONE',  ( -1.000000000000000000, -0.000000000000000000, -0.000000000000000000 ) ) ;
#10124 = LINE ( 'NONE', #11172, #12511 ) ;
#10125 = VECTOR ( 'NONE', #7647, 1000.000000000000000 ) ;
#10126 = ORIENTED_EDGE ( 'NONE', *, *, #9257, .T. ) ;
#10127 = VECTOR ( 'NONE', #12561, 1000.000000000000114 ) ;
#10128 = ORIENTED_EDGE ( 'NONE', *, *, #6342, .T. ) ;
#10129 = CARTESIAN_POINT ( 'NONE',  ( 17.49999999999998579, 90.00000000000002842, -10.00000000000000000 ) ) ;
#10130 = ORIENTED_EDGE ( 'NONE', *, *, #8672, .F. ) ;
#10131 = APPLICATION_PROTOCOL_DEFINITION ( 'draft international standard', 'automotive_design', 1998, #10180 ) ;
#10132 = CARTESIAN_POINT ( 'NONE',  ( 3.556430356250015024, 90.00000000000000000, 3.903125000614517504 ) ) ;
#10133 = VERTEX_POINT ( 'NONE', #8097 ) ;
#10134 = AXIS2_PLACEMENT_3D ( 'NONE', #4815, #1933, #2001 ) ;
#10135 = FACE_OUTER_BOUND ( 'NONE', #1055, .T. ) ;
#10136 = CARTESIAN_POINT ( 'NONE',  ( 52.49999999999996447, 86.00000000000000000, -10.00000000000000000 ) ) ;
#10137 = EDGE_LOOP ( 'NONE', ( #8503, #11542, #782, #2750 ) ) ;
#10138 = EDGE_CURVE ( 'NONE', #3551, #7582, #5535, .T. ) ;
#10139 = AXIS2_PLACEMENT_3D ( 'NONE', #7799, #2840, #6815 ) ;
#10140 = CARTESIAN_POINT ( 'NONE',  ( 7.500000000000000000, 35.90129092583966752, 0.000000000000000000 ) ) ;
#10141 = CARTESIAN_POINT ( 'NONE',  ( 35.00000000000000711, 53.69209320379639649, 4.015625000614517326 ) ) ;
#10142 = FACE_OUTER_BOUND ( 'NONE', #9207, .T. ) ;
#10143 = CARTESIAN_POINT ( 'NONE',  ( 3.800000000000025135, 71.98667160128366049, 2.900000001229034563 ) ) ;
#10144 = SURFACE_STYLE_USAGE ( .BOTH. , #9779 ) ;
#10145 = AXIS2_PLACEMENT_3D ( 'NONE', #10431, #6627, #4417 ) ;
#10146 = PLANE ( 'NONE',  #1658 ) ;
#10147 = EDGE_CURVE ( 'NONE', #8074, #454, #7504, .T. ) ;
#10149 = ADVANCED_FACE ( 'NONE', ( #2600 ), #6320, .F. ) ;
#10148 = ORIENTED_EDGE ( 'NONE', *, *, #9554, .F. ) ;
#10150 = AXIS2_PLACEMENT_3D ( 'NONE', #7374, #3272, #11362 ) ;
#10151 = CARTESIAN_POINT ( 'NONE',  ( 66.19999999999997442, 108.0133283987163253, 3.912500000000000533 ) ) ;
#10152 = ORIENTED_EDGE ( 'NONE', *, *, #9554, .T. ) ;
#10153 = CARTESIAN_POINT ( 'NONE',  ( 3.800000000000015365, 90.00000000000000000, 3.200000000000000178 ) ) ;
#10154 = EDGE_LOOP ( 'NONE', ( #3481, #1429, #9916 ) ) ;
#10155 = DIRECTION ( 'NONE',  ( 1.000000000000000000, 0.000000000000000000, 0.000000000000000000 ) ) ;
#10156 = ORIENTED_EDGE ( 'NONE', *, *, #8793, .F. ) ;
#10157 = DIRECTION ( 'NONE',  ( -0.000000000000000000, -0.000000000000000000, -1.000000000000000000 ) ) ;
#10158 = EDGE_CURVE ( 'NONE', #7369, #9537, #10382, .T. ) ;
#10159 = CARTESIAN_POINT ( 'NONE',  ( 35.00000000000000711, 53.69209320379640360, 4.015625000614517326 ) ) ;
#10160 = ORIENTED_EDGE ( 'NONE', *, *, #4286, .T. ) ;
#10161 = CARTESIAN_POINT ( 'NONE',  ( 3.556430356250015024, 90.00000000000000000, 3.509375000614517681 ) ) ;
#10162 = CARTESIAN_POINT ( 'NONE',  ( 44.16515138991168499, 94.00000000000000000, -8.000000000000000000 ) ) ;
#10163 = CARTESIAN_POINT ( 'NONE',  ( 0.000000000000000000, 0.000000000000000000, -0.8000000000000000444 ) ) ;
#10164 = CARTESIAN_POINT ( 'NONE',  ( -0.1325741768533960085, -4.273461295629625845, -0.8000000000000000444 ) ) ;
#10165 = PRODUCT_DEFINITION ( 'UNKNOWN', '', #3849, #3210 ) ;
#10166 = FACE_OUTER_BOUND ( 'NONE', #6191, .T. ) ;
#10167 = CARTESIAN_POINT ( 'NONE',  ( 35.00000000000000000, 90.00000000000000000, 4.800000000000000711 ) ) ;
#10168 = AXIS2_PLACEMENT_3D ( 'NONE', #10172, #4165, #10238 ) ;
#10169 = DIRECTION ( 'NONE',  ( 0.000000000000000000, -1.000000000000000000, 0.000000000000000000 ) ) ;
#10170 = EDGE_CURVE ( 'NONE', #11127, #1353, #8363, .T. ) ;
#10171 = CARTESIAN_POINT ( 'NONE',  ( 36.50000000000001421, 67.79999999999999716, 8.000000000000000000 ) ) ;
#10172 = CARTESIAN_POINT ( 'NONE',  ( 51.64126381929429499, 66.24461453698036451, 4.000000000000000000 ) ) ;
#10173 = VERTEX_POINT ( 'NONE', #7371 ) ;
#10174 = CARTESIAN_POINT ( 'NONE',  ( 3.033375984251970081, -8.673617379884035472E-16, 0.000000000000000000 ) ) ;
#10175 = VERTEX_POINT ( 'NONE', #10314 ) ;
#10176 = AXIS2_PLACEMENT_3D ( 'NONE', #2834, #10805, #7927 ) ;
#10177 = DIRECTION ( 'NONE',  ( 0.8660254037844395958, 0.4999999999999985567, 0.000000000000000000 ) ) ;
#10178 = CARTESIAN_POINT ( 'NONE',  ( 4.336808689942017736E-16, 0.000000000000000000, 0.000000000000000000 ) ) ;
#10179 = CARTESIAN_POINT ( 'NONE',  ( -61.00000000000000711, 31.73205080756887142, -0.9999999999999931166 ) ) ;
#10180 = APPLICATION_CONTEXT ( 'automotive_design' ) ;
#10181 = CARTESIAN_POINT ( 'NONE',  ( 17.55231228847961944, 66.83584248194507893, 2.000000000000002220 ) ) ;
#10182 = ORIENTED_EDGE ( 'NONE', *, *, #2697, .F. ) ;
#10183 = LINE ( 'NONE', #12150, #4713 ) ;
#10184 = EDGE_CURVE ( 'NONE', #7916, #12941, #194, .T. ) ;
#10185 = CARTESIAN_POINT ( 'NONE',  ( 44.16515138991168499, 94.00000000000000000, -18.00000000000000355 ) ) ;
#10186 = AXIS2_PLACEMENT_3D ( 'NONE', #3043, #74, #3177 ) ;
#10187 = ORIENTED_EDGE ( 'NONE', *, *, #3059, .T. ) ;
#10188 = DIRECTION ( 'NONE',  ( -1.000000000000000000, -0.000000000000000000, -0.000000000000000000 ) ) ;
#10189 = ORIENTED_EDGE ( 'NONE', *, *, #10929, .T. ) ;
#10190 = FILL_AREA_STYLE_COLOUR ( '', #1708 ) ;
#10191 = EDGE_LOOP ( 'NONE', ( #10300, #2163, #9038 ) ) ;
#10192 = CARTESIAN_POINT ( 'NONE',  ( 66.19999999999998863, 90.00000000000000000, 4.437500001229033764 ) ) ;
#10193 = CARTESIAN_POINT ( 'NONE',  ( -18.33333333333332504, 30.00000000000000000, 7.999999999999996447 ) ) ;
#10194 = AXIS2_PLACEMENT_3D ( 'NONE', #6782, #950, #12934 ) ;
#10195 = ORIENTED_EDGE ( 'NONE', *, *, #5709, .T. ) ;
#10196 = AXIS2_PLACEMENT_3D ( 'NONE', #9114, #11073, #10032 ) ;
#10197 = ADVANCED_FACE ( 'NONE', ( #2344 ), #9533, .F. ) ;
#10198 = ORIENTED_EDGE ( 'NONE', *, *, #8938, .F. ) ;
#10199 = CARTESIAN_POINT ( 'NONE',  ( 21.49999999999998579, 90.00000000000000000, -8.000000000000000000 ) ) ;
#10200 = ORIENTED_EDGE ( 'NONE', *, *, #5145, .F. ) ;
#10201 = ADVANCED_FACE ( 'NONE', ( #6449 ), #1481, .T. ) ;
#10202 = CARTESIAN_POINT ( 'NONE',  ( 66.44356964374998142, 108.1539533981018053, 4.615625000614516971 ) ) ;
#10203 = ORIENTED_EDGE ( 'NONE', *, *, #10639, .F. ) ;
#10204 = FACE_OUTER_BOUND ( 'NONE', #3719, .T. ) ;
#10205 = PLANE ( 'NONE',  #3961 ) ;
#10206 = EDGE_LOOP ( 'NONE', ( #8197, #7719, #6567, #12186 ) ) ;
#10207 = AXIS2_PLACEMENT_3D ( 'NONE', #5544, #1749, #3662 ) ;
#10208 = DIRECTION ( 'NONE',  ( -0.8660254037844359321, -0.5000000000000046629, -0.000000000000000000 ) ) ;
#10209 = CARTESIAN_POINT ( 'NONE',  ( 35.00000000000000711, 53.69209320379639649, 3.565625000614517592 ) ) ;
#10210 = DIRECTION ( 'NONE',  ( 0.000000000000000000, -1.000000000000000000, -0.000000000000000000 ) ) ;
#10211 = LINE ( 'NONE', #1047, #7268 ) ;
#10212 =( NAMED_UNIT ( * ) PLANE_ANGLE_UNIT ( ) SI_UNIT ( $, .RADIAN. ) );
#10213 = DIRECTION ( 'NONE',  ( 0.9510565162951543083, -0.3090169943749451198, 0.000000000000000000 ) ) ;
#10214 = EDGE_CURVE ( 'NONE', #6389, #8617, #5466, .T. ) ;
#10215 = AXIS2_PLACEMENT_3D ( 'NONE', #4410, #463, #3501 ) ;
#10216 = VERTEX_POINT ( 'NONE', #12478 ) ;
#10217 = CARTESIAN_POINT ( 'NONE',  ( 35.00000000000000000, 126.0266567974326222, 3.987499999999999378 ) ) ;
#10218 = ORIENTED_EDGE ( 'NONE', *, *, #10679, .F. ) ;
#10219 = LINE ( 'NONE', #6091, #605 ) ;
#10220 = EDGE_LOOP ( 'NONE', ( #12702, #7037, #10336, #9007 ) ) ;
#10221 = EDGE_CURVE ( 'NONE', #3473, #3079, #3458, .T. ) ;
#10222 = DIRECTION ( 'NONE',  ( -5.624500927088228034E-17, 1.370729058197317968E-18, 1.000000000000000000 ) ) ;
#10223 = ORIENTED_EDGE ( 'NONE', *, *, #1049, .F. ) ;
#10224 = CARTESIAN_POINT ( 'NONE',  ( 0.000000000000000000, 0.000000000000000000, -0.8000000000000000444 ) ) ;
#10225 = CARTESIAN_POINT ( 'NONE',  ( 66.44356964374998142, 108.1539533981018053, 3.715625000614517948 ) ) ;
#10226 = CIRCLE ( 'NONE', #4795, 2.396199811936270407 ) ;
#10227 = EDGE_CURVE ( 'NONE', #4781, #3479, #7732, .T. ) ;
#10228 = CARTESIAN_POINT ( 'NONE',  ( 19.27821517812500574, 117.2309300971526937, 3.434375000614517059 ) ) ;
#10229 = CARTESIAN_POINT ( 'NONE',  ( 1.040000000000000036, 1.154700538379252350, 7.017607234860990640E-28 ) ) ;
#10230 = DIRECTION ( 'NONE',  ( -1.000000000000000000, -0.000000000000000000, -0.000000000000000000 ) ) ;
#10231 = AXIS2_PLACEMENT_3D ( 'NONE', #5146, #7968, #12021 ) ;
#10232 = DIRECTION ( 'NONE',  ( 1.000000000000000000, 0.000000000000000000, 8.673617379884034486E-16 ) ) ;
#10233 = CARTESIAN_POINT ( 'NONE',  ( -28.99038105676692112, 50.21281292110204930, 1.000000000000000000 ) ) ;
#10234 = FACE_OUTER_BOUND ( 'NONE', #1556, .T. ) ;
#10235 = FACE_OUTER_BOUND ( 'NONE', #5147, .T. ) ;
#10236 = DIRECTION ( 'NONE',  ( 0.000000000000000000, 0.000000000000000000, -1.000000000000000000 ) ) ;
#10237 = B_SPLINE_CURVE_WITH_KNOTS ( 'NONE', 3,
 ( #11859, #10874, #1918, #9891, #12908, #11923, #5963, #10686, #9702, #12719, #7743, #10748, #9412, #3408, #7080, #373, #9350, #906, #6092, #64, #4018, #5112, #8001, #12427, #11984, #2116, #2049, #3031, #6400, #4080, #6028, #4384, #1430, #129, #437, #10023, #8068, #10398 ),
 .UNSPECIFIED., .F., .F.,
 ( 4, 2, 2, 2, 2, 2, 2, 2, 2, 2, 2, 2, 2, 2, 2, 2, 2, 2, 4 ),
 ( 0.000000000000000000, 0.001940799028833090425, 0.003881598057666180851, 0.007763196115332329610, 0.01164479417299847663, 0.01552639223066462452, 0.02328958834599692898, 0.02523038737482999685, 0.02717118640366306126, 0.03105278446132919354, 0.03299358349016226488, 0.03493438251899534663, 0.03881598057666148932, 0.04269757863432762507, 0.04463837766316068600, 0.04657917669199374694, 0.05046077474965985493, 0.05434237280732596292, 0.06210556892265813728 ),
 .UNSPECIFIED. ) ;
#10238 = DIRECTION ( 'NONE',  ( 0.5877852522924753575, -0.8090169943749457859, 0.000000000000000000 ) ) ;
#10240 = ADVANCED_FACE ( 'NONE', ( #10509 ), #5401, .T. ) ;
#10239 = EDGE_LOOP ( 'NONE', ( #12426, #2537, #240, #5540 ) ) ;
#10241 = EDGE_CURVE ( 'NONE', #7119, #5860, #7939, .T. ) ;
#10242 = VECTOR ( 'NONE', #10236, 1000.000000000000000 ) ;
#10243 = LINE ( 'NONE', #11614, #5586 ) ;
#10244 = ORIENTED_EDGE ( 'NONE', *, *, #11304, .F. ) ;
#10245 = CARTESIAN_POINT ( 'NONE',  ( 4.763019983628629994, -4.349268977144817860, -0.8000000000000000444 ) ) ;
#10246 = CARTESIAN_POINT ( 'NONE',  ( 3.800000000000015365, 90.00000000000000000, 4.549999999999999822 ) ) ;
#10247 = DIRECTION ( 'NONE',  ( -0.000000000000000000, -1.000000000000000000, -0.000000000000000000 ) ) ;
#10248 = AXIS2_PLACEMENT_3D ( 'NONE', #8202, #4405, #7218 ) ;
#10249 = VERTEX_POINT ( 'NONE', #7567 ) ;
#10250 = DIRECTION ( 'NONE',  ( -1.000000000000000000, 0.000000000000000000, 0.000000000000000000 ) ) ;
#10251 = ORIENTED_EDGE ( 'NONE', *, *, #3895, .T. ) ;
#10252 = DIRECTION ( 'NONE',  ( 1.000000000000000000, 0.000000000000000000, 0.000000000000000000 ) ) ;
#10253 = CARTESIAN_POINT ( 'NONE',  ( 8.500000000000000000, 71.85789451624832225, 3.000000000000000000 ) ) ;
#10254 = VERTEX_POINT ( 'NONE', #11554 ) ;
#10255 = PRODUCT_DEFINITION ( 'UNKNOWN', '', #2178, #6205 ) ;
#10256 = VERTEX_POINT ( 'NONE', #421 ) ;
#10257 = CARTESIAN_POINT ( 'NONE',  ( 35.00000000000000000, 126.0266567974326222, 2.750000001229034208 ) ) ;
#10258 = AXIS2_PLACEMENT_3D ( 'NONE', #8138, #2911, #12849 ) ;
#10259 = DIRECTION ( 'NONE',  ( 0.000000000000000000, 0.000000000000000000, 1.000000000000000000 ) ) ;
#10260 = EDGE_CURVE ( 'NONE', #4053, #7731, #1494, .T. ) ;
#10261 = VERTEX_POINT ( 'NONE', #5603 ) ;
#10262 = VERTEX_POINT ( 'NONE', #10699 ) ;
#10263 = DIRECTION ( 'NONE',  ( 1.000000000000000000, 0.000000000000000000, 0.000000000000000000 ) ) ;
#10264 = VERTEX_POINT ( 'NONE', #11622 ) ;
#10265 = CARTESIAN_POINT ( 'NONE',  ( 50.72178482187499071, 117.2309300971526937, 2.853125000614517237 ) ) ;
#10266 = ORIENTED_EDGE ( 'NONE', *, *, #4858, .T. ) ;
#10267 = CIRCLE ( 'NONE', #853, 4.338286831716297698 ) ;
#10268 = CARTESIAN_POINT ( 'NONE',  ( 10.16381611175368604, 72.81849919625140899, -1.000000000000000000 ) ) ;
#10269 = VERTEX_POINT ( 'NONE', #12673 ) ;
#10270 = ADVANCED_BREP_SHAPE_REPRESENTATION ( '', ( #12002, #5704 ), #12825 ) ;
#10271 = FACE_OUTER_BOUND ( 'NONE', #5481, .T. ) ;
#10272 = ADVANCED_FACE ( 'NONE', ( #7696 ), #6708, .F. ) ;
#10273 = CARTESIAN_POINT ( 'NONE',  ( 0.000000000000000000, 30.00000000000000000, 0.000000000000000000 ) ) ;
#10274 = CARTESIAN_POINT ( 'NONE',  ( 50.59999999999999432, 117.0199925980744666, 2.712500001229034119 ) ) ;
#10275 = EDGE_CURVE ( 'NONE', #1184, #585, #11817, .T. ) ;
#10276 = SURFACE_SIDE_STYLE ('',( #8388 ) ) ;
#10277 = VECTOR ( 'NONE', #7118, 1000.000000000000114 ) ;
#10278 = CARTESIAN_POINT ( 'NONE',  ( 3.800000000000001155, 108.0133283987163111, 4.512500000000001066 ) ) ;
#10279 = ORIENTED_EDGE ( 'NONE', *, *, #10389, .T. ) ;
#10280 = CARTESIAN_POINT ( 'NONE',  ( 3.556430356250015024, 90.00000000000000000, 4.409375000614517148 ) ) ;
#10281 = EDGE_LOOP ( 'NONE', ( #560, #9706, #5084, #11040 ) ) ;
#10282 = CARTESIAN_POINT ( 'NONE',  ( -48.33333333333332860, 2.000000000000000000, -1.734723475976807094E-15 ) ) ;
#10283 = ORIENTED_EDGE ( 'NONE', *, *, #10948, .T. ) ;
#10284 = CARTESIAN_POINT ( 'NONE',  ( 21.49999999999998579, 90.00000000000000000, -5.000000000000000000 ) ) ;
#10285 = VERTEX_POINT ( 'NONE', #2795 ) ;
#10286 = VECTOR ( 'NONE', #8595, 1000.000000000000000 ) ;
#10287 = CARTESIAN_POINT ( 'NONE',  ( 1.040000000000000036, 0.5773502691896262862, 1.000000000000000000 ) ) ;
#10288 = CARTESIAN_POINT ( 'NONE',  ( 5.500109330110817041, 100.8955221554261072, 2.999999999999999112 ) ) ;
#10289 = EDGE_CURVE ( 'NONE', #3204, #4892, #1742, .T. ) ;
#10290 = CARTESIAN_POINT ( 'NONE',  ( 3.556430356250014579, 108.1539533981018053, 3.471875000614516704 ) ) ;
#10291 = CARTESIAN_POINT ( 'NONE',  ( 7.500000000000000000, 30.00000000000000000, -1.599999999999992095 ) ) ;
#10292 = CARTESIAN_POINT ( 'NONE',  ( 4.338286831716297698, 0.4117131682837005258, 0.000000000000000000 ) ) ;
#10293 = VECTOR ( 'NONE', #7639, 999.9999999999998863 ) ;
#10294 =( NAMED_UNIT ( * ) PLANE_ANGLE_UNIT ( ) SI_UNIT ( $, .RADIAN. ) );
#10295 = CYLINDRICAL_SURFACE ( 'NONE', #7085, 4.000000000000003553 ) ;
#10296 = LINE ( 'NONE', #4096, #3019 ) ;
#10297 = PLANE ( 'NONE',  #3477 ) ;
#10298 = DIRECTION ( 'NONE',  ( -1.000000000000000000, -9.570888143320317860E-16, 0.000000000000000000 ) ) ;
#10299 = CARTESIAN_POINT ( 'NONE',  ( 3.556430356250028790, 71.84604660189818048, 3.096875000614517148 ) ) ;
#10300 = ORIENTED_EDGE ( 'NONE', *, *, #4971, .F. ) ;
#10301 = ADVANCED_FACE ( 'NONE', ( #3589 ), #2735, .F. ) ;
#10302 =( GEOMETRIC_REPRESENTATION_CONTEXT ( 3 ) GLOBAL_UNCERTAINTY_ASSIGNED_CONTEXT ( ( #8583 ) ) GLOBAL_UNIT_ASSIGNED_CONTEXT ( ( #7431, #1609, #615 ) ) REPRESENTATION_CONTEXT ( 'NONE', 'WORKASPACE' ) );
#10303 = DIRECTION ( 'NONE',  ( 0.000000000000000000, 0.000000000000000000, 1.000000000000000000 ) ) ;
#10304 = ORIENTED_EDGE ( 'NONE', *, *, #9543, .F. ) ;
#10305 =( NAMED_UNIT ( * ) SI_UNIT ( $, .STERADIAN. ) SOLID_ANGLE_UNIT ( ) );
#10306 = VECTOR ( 'NONE', #9985, 1000.000000000000000 ) ;
#10307 = LINE ( 'NONE', #2339, #6358 ) ;
#10308 = DIRECTION ( 'NONE',  ( 0.000000000000000000, 0.000000000000000000, 1.000000000000000000 ) ) ;
#10309 = EDGE_CURVE ( 'NONE', #10133, #7510, #8618, .T. ) ;
#10310 = DIRECTION ( 'NONE',  ( -0.8090169943749457859, -0.5877852522924753575, 0.000000000000000000 ) ) ;
#10311 = EDGE_CURVE ( 'NONE', #8478, #6336, #6901, .T. ) ;
#10312 = ORIENTED_EDGE ( 'NONE', *, *, #7274, .F. ) ;
#10313 = CARTESIAN_POINT ( 'NONE',  ( 52.22659979626836702, 65.43896868087158225, 1.000000000000003109 ) ) ;
#10314 = CARTESIAN_POINT ( 'NONE',  ( 66.19999999999998863, 90.00000000000000000, 3.425000000000000266 ) ) ;
#10315 = ORIENTED_EDGE ( 'NONE', *, *, #6595, .F. ) ;
#10316 =( LENGTH_UNIT ( ) NAMED_UNIT ( * ) SI_UNIT ( .MILLI., .METRE. ) );
#10317 = CIRCLE ( 'NONE', #2593, 0.7499999999999997780 ) ;
#10318 = CARTESIAN_POINT ( 'NONE',  ( 66.20000000000000284, 90.00000000000000000, -8.000000000000000000 ) ) ;
#10319 = EDGE_LOOP ( 'NONE', ( #9267, #7773, #10394, #8941 ) ) ;
#10320 = EDGE_CURVE ( 'NONE', #8524, #10256, #9721, .T. ) ;
#10321 = ORIENTED_EDGE ( 'NONE', *, *, #5434, .T. ) ;
#10322 = CARTESIAN_POINT ( 'NONE',  ( 50.59999999999999432, 117.0199925980744666, 2.712500001229034119 ) ) ;
#10323 = AXIS2_PLACEMENT_3D ( 'NONE', #9535, #6261, #10252 ) ;
#10324 = CARTESIAN_POINT ( 'NONE',  ( 46.99999999999995737, 90.00000000000000000, -5.000000000000000000 ) ) ;
#10325 = EDGE_LOOP ( 'NONE', ( #5754, #2053, #1173, #3558, #7987 ) ) ;
#10326 = VECTOR ( 'NONE', #10763, 1000.000000000000000 ) ;
#10327 = PRODUCT_DEFINITION_SHAPE ( 'NONE', 'NONE',  #3872 ) ;
#10328 = VERTEX_POINT ( 'NONE', #6581 ) ;
#10329 = AXIS2_PLACEMENT_3D ( 'NONE', #7029, #8863, #2918 ) ;
#10330 = DIRECTION ( 'NONE',  ( 0.000000000000000000, 1.224646799147353207E-16, -1.000000000000000000 ) ) ;
#10331 = PRODUCT_RELATED_PRODUCT_CATEGORY ( 'part', '', ( #11480 ) ) ;
#10332 = ORIENTED_EDGE ( 'NONE', *, *, #12440, .T. ) ;
#10333 = CARTESIAN_POINT ( 'NONE',  ( -1.436050757534458100, -5.516136167806656943, -0.8000000000000000444 ) ) ;
#10334 = PRODUCT_CONTEXT ( 'NONE', #4174, 'mechanical' ) ;
#10335 = CARTESIAN_POINT ( 'NONE',  ( 64.31840935109022439, 100.6710296186405600, 2.661976390793298286 ) ) ;
#10336 = ORIENTED_EDGE ( 'NONE', *, *, #12589, .T. ) ;
#10337 = EDGE_CURVE ( 'NONE', #5076, #58, #10768, .T. ) ;
#10338 = PLANE ( 'NONE',  #11464 ) ;
#10339 = ORIENTED_EDGE ( 'NONE', *, *, #10046, .F. ) ;
#10340 = CARTESIAN_POINT ( 'NONE',  ( 25.00000000000000355, -5.901290925839664858, -5.750000000000000000 ) ) ;
#10341 = VECTOR ( 'NONE', #2553, 1000.000000000000114 ) ;
#10342 = AXIS2_PLACEMENT_3D ( 'NONE', #11586, #386, #12508 ) ;
#10343 = DIRECTION ( 'NONE',  ( -1.000000000000000000, -0.000000000000000000, -0.000000000000000000 ) ) ;
#10344 = CARTESIAN_POINT ( 'NONE',  ( 0.1999999999999965694, -6.446898479113814417, 0.000000000000000000 ) ) ;
#10345 = ORIENTED_EDGE ( 'NONE', *, *, #2250, .F. ) ;
#10346 = CARTESIAN_POINT ( 'NONE',  ( 19.27821517812503060, 62.76906990284727783, 3.134375000614517237 ) ) ;
#10347 = ADVANCED_FACE ( 'NONE', ( #2669 ), #6645, .T. ) ;
#10348 = ORIENTED_EDGE ( 'NONE', *, *, #4443, .T. ) ;
#10349 = VECTOR ( 'NONE', #9134, 1000.000000000000000 ) ;
#10350 = CARTESIAN_POINT ( 'NONE',  ( -60.00000000000000000, -6.000000000000000000, -15.00000000000000355 ) ) ;
#10351 = VERTEX_POINT ( 'NONE', #3840 ) ;
#10352 = CIRCLE ( 'NONE', #12655, 6.499999999999999112 ) ;
#10353 = CARTESIAN_POINT ( 'NONE',  ( 66.44356964374999563, 90.00000000000000000, 4.184375000614516615 ) ) ;
#10354 = EDGE_CURVE ( 'NONE', #4104, #4463, #9597, .T. ) ;
#10355 = ORIENTED_EDGE ( 'NONE', *, *, #5724, .T. ) ;
#10356 = DIRECTION ( 'NONE',  ( -0.000000000000000000, -1.000000000000000000, -0.000000000000000000 ) ) ;
#10357 = CARTESIAN_POINT ( 'NONE',  ( 6.061620567163541473, 102.3095278883966444, 3.000000000000001776 ) ) ;
#10358 = CARTESIAN_POINT ( 'NONE',  ( 50.72178482187499071, 117.2309300971526937, 3.809375000614517504 ) ) ;
#10359 = DIRECTION ( 'NONE',  ( -0.000000000000000000, -0.000000000000000000, -1.000000000000000000 ) ) ;
#10360 = CARTESIAN_POINT ( 'NONE',  ( 1.040000000000000036, 0.000000000000000000, 0.000000000000000000 ) ) ;
#10361 = PRESENTATION_LAYER_ASSIGNMENT (  '', '', ( #3052 ) ) ;
#10362 = DIRECTION ( 'NONE',  ( 1.000000000000000000, 0.000000000000000000, 0.000000000000000000 ) ) ;
#10363 = DIRECTION ( 'NONE',  ( 0.000000000000000000, 0.8660254037844384856, 0.5000000000000004441 ) ) ;
#10364 = EDGE_CURVE ( 'NONE', #10328, #2398, #1682, .T. ) ;
#10365 = CARTESIAN_POINT ( 'NONE',  ( 6.000000000000008882, 90.00000000000000000, 4.000000000000000000 ) ) ;
#10366 = LINE ( 'NONE', #11606, #11151 ) ;
#10367 = FACE_BOUND ( 'NONE', #8610, .T. ) ;
#10368 = AXIS2_PLACEMENT_3D ( 'NONE', #6323, #7248, #12222 ) ;
#10369 = CARTESIAN_POINT ( 'NONE',  ( 50.59999999999999432, 117.0199925980744666, 4.850000000000000533 ) ) ;
#10370 = LINE ( 'NONE', #5453, #2449 ) ;
#10371 = ORIENTED_EDGE ( 'NONE', *, *, #7988, .F. ) ;
#10372 = CARTESIAN_POINT ( 'NONE',  ( 35.00000000000000000, 90.00000000000000000, -3.799999999999999822 ) ) ;
#10373 = ORIENTED_EDGE ( 'NONE', *, *, #9075, .T. ) ;
#10374 =( NAMED_UNIT ( * ) SI_UNIT ( $, .STERADIAN. ) SOLID_ANGLE_UNIT ( ) );
#10375 = CIRCLE ( 'NONE', #8083, 6.499999999999999112 ) ;
#10376 = CYLINDRICAL_SURFACE ( 'NONE', #11662, 2.396199811936269963 ) ;
#10377 = DIRECTION ( 'NONE',  ( -1.000000000000000000, 0.000000000000000000, 0.000000000000000000 ) ) ;
#10378 = EDGE_CURVE ( 'NONE', #3935, #12624, #1873, .T. ) ;
#10379 = DIRECTION ( 'NONE',  ( 0.000000000000000000, 0.000000000000000000, -1.000000000000000000 ) ) ;
#10380 = VERTEX_POINT ( 'NONE', #9658 ) ;
#10381 = CARTESIAN_POINT ( 'NONE',  ( 48.49999999999995737, 90.00000000000000000, -8.000000000000000000 ) ) ;
#10382 = LINE ( 'NONE', #555, #5428 ) ;
#10383 = VERTEX_POINT ( 'NONE', #5858 ) ;
#10384 = CARTESIAN_POINT ( 'NONE',  ( 28.68194083117252902, 91.52713075379780605, 22.38477631085024555 ) ) ;
#10385 = EDGE_LOOP ( 'NONE', ( #8049, #3027 ) ) ;
#10386 = VECTOR ( 'NONE', #279, 1000.000000000000000 ) ;
#10387 = ORIENTED_EDGE ( 'NONE', *, *, #6796, .T. ) ;
#10388 = EDGE_CURVE ( 'NONE', #6517, #5066, #3778, .T. ) ;
#10389 = EDGE_CURVE ( 'NONE', #4807, #5354, #1617, .T. ) ;
#10390 = CARTESIAN_POINT ( 'NONE',  ( 35.00000000000000000, 126.0266567974326222, 4.550000001229034474 ) ) ;
#10391 = CARTESIAN_POINT ( 'NONE',  ( 34.49999999999998579, 96.48074069840785683, 4.000000000000000000 ) ) ;
#10392 = ORIENTED_EDGE ( 'NONE', *, *, #2366, .T. ) ;
#10393 = PRODUCT_DEFINITION_CONTEXT ( 'detailed design', #1590, 'design' ) ;
#10394 = ORIENTED_EDGE ( 'NONE', *, *, #5749, .T. ) ;
#10395 = CARTESIAN_POINT ( 'NONE',  ( 62.42613047537196991, 99.43702109502110886, 4.000000000000000000 ) ) ;
#10396 = ORIENTED_EDGE ( 'NONE', *, *, #5870, .T. ) ;
#10397 = EDGE_CURVE ( 'NONE', #1613, #4495, #8741, .T. ) ;
#10398 = CARTESIAN_POINT ( 'NONE',  ( 64.24207199149496716, 100.8784753363798075, 2.999999999999999556 ) ) ;
#10399 = ITEM_DEFINED_TRANSFORMATION ( 'NONE', 'NONE', #275,  #5704 ) ;
#10400 = CARTESIAN_POINT ( 'NONE',  ( 50.59999999999999432, 117.0199925980744666, 3.162500001229034741 ) ) ;
#10401 = ORIENTED_EDGE ( 'NONE', *, *, #10260, .T. ) ;
#10402 = DIRECTION ( 'NONE',  ( 8.673617379884034486E-16, 5.007715329123921945E-16, -1.000000000000000000 ) ) ;
#10403 = VERTEX_POINT ( 'NONE', #9786 ) ;
#10404 = LINE ( 'NONE', #7393, #6080 ) ;
#10405 = ORIENTED_EDGE ( 'NONE', *, *, #4526, .F. ) ;
#10406 = AXIS2_PLACEMENT_3D ( 'NONE', #7221, #5122, #11209 ) ;
#10407 = EDGE_CURVE ( 'NONE', #4788, #1482, #10701, .T. ) ;
#10408 = CARTESIAN_POINT ( 'NONE',  ( 66.20000000000008811, 108.0133283987162542, 3.125000001229034208 ) ) ;
#10409 = CARTESIAN_POINT ( 'NONE',  ( 1.040000000000000036, -0.5773502691896253980, -1.000000000000000000 ) ) ;
#10410 = FILL_AREA_STYLE ('',( #2438 ) ) ;
#10411 = ORIENTED_EDGE ( 'NONE', *, *, #4903, .F. ) ;
#10412 = CARTESIAN_POINT ( 'NONE',  ( 39.21379230364324542, 85.05086326499692007, -0.9999999999999970024 ) ) ;
#10413 = ORIENTED_EDGE ( 'NONE', *, *, #9316, .F. ) ;
#10414 = VECTOR ( 'NONE', #8091, 1000.000000000000000 ) ;
#10415 = CARTESIAN_POINT ( 'NONE',  ( 5.000000000000004441, 30.00000000000000000, 2.500000000000000444 ) ) ;
#10416 = AXIS2_PLACEMENT_3D ( 'NONE', #4377, #3341, #11238 ) ;
#10417 = CARTESIAN_POINT ( 'NONE',  ( 66.44356964374999563, 71.84604660189820891, 4.146875000614517859 ) ) ;
#10418 = VERTEX_POINT ( 'NONE', #3714 ) ;
#10419 = CARTESIAN_POINT ( 'NONE',  ( -6.666666666666660745, 0.000000000000000000, 1.599999999999998090 ) ) ;
#10420 = CARTESIAN_POINT ( 'NONE',  ( 31.96709571323326671, 88.25314809233525182, -3.000000000000000888 ) ) ;
#10421 = CARTESIAN_POINT ( 'NONE',  ( 3.556430356250015024, 90.00000000000000000, 3.509375000614517681 ) ) ;
#10422 = LINE ( 'NONE', #11530, #12504 ) ;
#10424 = VECTOR ( 'NONE', #6102, 1000.000000000000114 ) ;
#10423 = CARTESIAN_POINT ( 'NONE',  ( 31.50000000000000000, 90.00000000000000000, -3.799999999999999378 ) ) ;
#10425 = DIRECTION ( 'NONE',  ( -0.9510565162951543083, 0.3090169943749451198, 0.000000000000000000 ) ) ;
#10426 = EDGE_CURVE ( 'NONE', #12446, #255, #8581, .T. ) ;
#10427 = CARTESIAN_POINT ( 'NONE',  ( 17.26299177799148055, 43.12143982588584379, -0.9999999999999970024 ) ) ;
#10428 = FACE_OUTER_BOUND ( 'NONE', #10220, .T. ) ;
#10429 = DIRECTION ( 'NONE',  ( 1.000000000000000000, 1.914177628664063178E-15, -0.000000000000000000 ) ) ;
#10430 = AXIS2_PLACEMENT_3D ( 'NONE', #5517, #12591, #2906 ) ;
#10431 = CARTESIAN_POINT ( 'NONE',  ( 45.00000000000000000, -5.000000000000000000, 5.750000000000000888 ) ) ;
#10432 = DIRECTION ( 'NONE',  ( -0.000000000000000000, 0.000000000000000000, -1.000000000000000000 ) ) ;
#10433 = LINE ( 'NONE', #11541, #10796 ) ;
#10434 = VERTEX_POINT ( 'NONE', #814 ) ;
#10435 = CARTESIAN_POINT ( 'NONE',  ( -18.33333333333332504, 46.12451549659709116, -7.999999999999996447 ) ) ;
#10436 = DIRECTION ( 'NONE',  ( -0.000000000000000000, 1.000000000000000000, -0.000000000000000000 ) ) ;
#10437 = ORIENTED_EDGE ( 'NONE', *, *, #4845, .T. ) ;
#10438 = EDGE_CURVE ( 'NONE', #5034, #85, #1266, .T. ) ;
#10439 = AXIS2_PLACEMENT_3D ( 'NONE', #10996, #2777, #5841 ) ;
#10440 = EDGE_CURVE ( 'NONE', #1516, #8153, #10582, .T. ) ;
#10441 = FACE_OUTER_BOUND ( 'NONE', #3951, .T. ) ;
#10442 = LINE ( 'NONE', #1411, #523 ) ;
#10443 = FACE_BOUND ( 'NONE', #9212, .T. ) ;
#10444 = VERTEX_POINT ( 'NONE', #7035 ) ;
#10445 = CARTESIAN_POINT ( 'NONE',  ( 35.00000000000000000, 90.00000000000000000, 4.800000000000000711 ) ) ;
#10446 = CARTESIAN_POINT ( 'NONE',  ( 12.55092940903992549, 109.9007343985615393, -3.000000000000000000 ) ) ;
#10447 = ORIENTED_EDGE ( 'NONE', *, *, #8393, .F. ) ;
#10448 = VECTOR ( 'NONE', #11639, 1000.000000000000114 ) ;
#10449 =( NAMED_UNIT ( * ) PLANE_ANGLE_UNIT ( ) SI_UNIT ( $, .RADIAN. ) );
#10450 = DIRECTION ( 'NONE',  ( 0.8660254037844361541, 0.5000000000000042188, 0.000000000000000000 ) ) ;
#10451 = ORIENTED_EDGE ( 'NONE', *, *, #1230, .F. ) ;
#10452 = FACE_OUTER_BOUND ( 'NONE', #3493, .T. ) ;
#10453 = ORIENTED_EDGE ( 'NONE', *, *, #3925, .T. ) ;
#10454 = ADVANCED_FACE ( 'NONE', ( #9123 ), #7955, .T. ) ;
#10455 = CARTESIAN_POINT ( 'NONE',  ( -67.46410161513773573, 36.92820323027551410, 2.500000000000000000 ) ) ;
#10456 = FACE_OUTER_BOUND ( 'NONE', #9127, .T. ) ;
#10457 = EDGE_LOOP ( 'NONE', ( #7507, #7491, #6113, #3937 ) ) ;
#10458 = CIRCLE ( 'NONE', #10871, 0.1000000000000000472 ) ;
#10459 = VERTEX_POINT ( 'NONE', #12926 ) ;
#10460 = DIRECTION ( 'NONE',  ( 1.000000000000000000, 0.000000000000000000, 0.000000000000000000 ) ) ;
#10461 = ORIENTED_EDGE ( 'NONE', *, *, #1979, .F. ) ;
#10462 = DIRECTION ( 'NONE',  ( 0.000000000000000000, 0.000000000000000000, 1.000000000000000000 ) ) ;
#10463 = CONTEXT_DEPENDENT_SHAPE_REPRESENTATION ( #8773, #11185 ) ;
#10464 = CARTESIAN_POINT ( 'NONE',  ( 50.60000000000001563, 62.98000740192552627, 3.012500001229034829 ) ) ;
#10465 = ORIENTED_EDGE ( 'NONE', *, *, #5511, .T. ) ;
#10466 = VERTEX_POINT ( 'NONE', #5914 ) ;
#10467 = VECTOR ( 'NONE', #12660, 1000.000000000000227 ) ;
#10468 = PLANE ( 'NONE',  #7349 ) ;
#10469 = ORIENTED_EDGE ( 'NONE', *, *, #1063, .T. ) ;
#10470 = CARTESIAN_POINT ( 'NONE',  ( 44.18196757760600235, 60.16945102741546947, 2.999999999999999112 ) ) ;
#10471 = DIRECTION ( 'NONE',  ( 0.000000000000000000, 0.000000000000000000, -1.000000000000000000 ) ) ;
#10472 = ORIENTED_EDGE ( 'NONE', *, *, #12514, .T. ) ;
#10473 = VECTOR ( 'NONE', #8653, 1000.000000000000000 ) ;
#10474 = CARTESIAN_POINT ( 'NONE',  ( 50.72178482187499071, 117.2309300971526937, 3.359375000614517326 ) ) ;
#10475 = VERTEX_POINT ( 'NONE', #6966 ) ;
#10476 = EDGE_CURVE ( 'NONE', #8117, #11802, #11082, .T. ) ;
#10477 = DIRECTION ( 'NONE',  ( -0.000000000000000000, -1.000000000000000000, 0.000000000000000000 ) ) ;
#10478 = ADVANCED_FACE ( 'NONE', ( #10103 ), #11937, .T. ) ;
#10479 = ORIENTED_EDGE ( 'NONE', *, *, #9714, .F. ) ;
#10480 = CARTESIAN_POINT ( 'NONE',  ( 35.00000000000000000, 126.3079067962035822, 4.746875000614517504 ) ) ;
#10481 = ORIENTED_EDGE ( 'NONE', *, *, #10558, .F. ) ;
#10482 = PLANE ( 'NONE',  #7337 ) ;
#10483 = LINE ( 'NONE', #11596, #6609 ) ;
#10484 = CARTESIAN_POINT ( 'NONE',  ( 3.556430356250015024, 90.00000000000000000, 4.409375000614517148 ) ) ;
#10485 = VECTOR ( 'NONE', #9451, 1000.000000000000000 ) ;
#10486 = CARTESIAN_POINT ( 'NONE',  ( 19.27821517812503060, 62.76906990284727783, 4.428125000614516971 ) ) ;
#10487 = CARTESIAN_POINT ( 'NONE',  ( 3.000000000000002665, 30.00000000000000000, -8.000000000000000000 ) ) ;
#10488 = DIRECTION ( 'NONE',  ( -0.000000000000000000, -1.000000000000000000, -0.000000000000000000 ) ) ;
#10489 = CARTESIAN_POINT ( 'NONE',  ( 25.83484861008832567, 94.00000000000000000, -8.000000000000000000 ) ) ;
#10490 = CARTESIAN_POINT ( 'NONE',  ( 35.75000000000000711, 93.41869858279433458, 4.000000000000000000 ) ) ;
#10491 = FACE_OUTER_BOUND ( 'NONE', #1650, .T. ) ;
#10492 = AXIS2_PLACEMENT_3D ( 'NONE', #446, #1376, #8447 ) ;
#10493 = CARTESIAN_POINT ( 'NONE',  ( 25.00000000000000355, 2.000000000000001332, 4.150000000000012790 ) ) ;
#10494 = DIRECTION ( 'NONE',  ( 0.000000000000000000, -1.224646799147353207E-16, 1.000000000000000000 ) ) ;
#10495 = LINE ( 'NONE', #1531, #7864 ) ;
#10496 = EDGE_CURVE ( 'NONE', #6062, #3535, #3118, .T. ) ;
#10497 = ORIENTED_EDGE ( 'NONE', *, *, #4395, .T. ) ;
#10498 = FACE_OUTER_BOUND ( 'NONE', #3677, .T. ) ;
#10499 = FACE_OUTER_BOUND ( 'NONE', #755, .T. ) ;
#10500 = ORIENTED_EDGE ( 'NONE', *, *, #1559, .F. ) ;
#10501 = FILL_AREA_STYLE ('',( #11481 ) ) ;
#10502 = AXIS2_PLACEMENT_3D ( 'NONE', #11839, #10974, #1093 ) ;
#10503 = CARTESIAN_POINT ( 'NONE',  ( -3.350000000000000089, 4.102566777143633281E-16, -0.8000000000000000444 ) ) ;
#10504 = CARTESIAN_POINT ( 'NONE',  ( 31.99902028769960438, 88.51116798584881451, -3.800000000000000266 ) ) ;
#10505 = CARTESIAN_POINT ( 'NONE',  ( 3.800000000000015365, 90.00000000000000000, 3.762500001229034385 ) ) ;
#10506 = ORIENTED_EDGE ( 'NONE', *, *, #8081, .T. ) ;
#10507 = ADVANCED_FACE ( 'NONE', ( #2133 ), #6109, .F. ) ;
#10508 = DIRECTION ( 'NONE',  ( 0.000000000000000000, -0.4999999999999998890, 0.8660254037844387076 ) ) ;
#10509 = FACE_OUTER_BOUND ( 'NONE', #6542, .T. ) ;
#10510 = ORIENTED_EDGE ( 'NONE', *, *, #6714, .T. ) ;
#10511 = VECTOR ( 'NONE', #5802, 1000.000000000000227 ) ;
#10512 = CARTESIAN_POINT ( 'NONE',  ( 0.000000000000000000, 0.000000000000000000, 0.000000000000000000 ) ) ;
#10513 = EDGE_CURVE ( 'NONE', #8267, #1018, #9911, .T. ) ;
#10514 = ORIENTED_EDGE ( 'NONE', *, *, #1524, .F. ) ;
#10515 = CARTESIAN_POINT ( 'NONE',  ( 66.20000000000008811, 108.0133283987162542, 4.362499999999998934 ) ) ;
#10516 = ORIENTED_EDGE ( 'NONE', *, *, #6307, .F. ) ;
#10517 = AXIS2_PLACEMENT_3D ( 'NONE', #8198, #9170, #12185 ) ;
#10518 = CARTESIAN_POINT ( 'NONE',  ( 30.78620769635677590, 85.05086326499690585, 4.000000000000000000 ) ) ;
#10519 = DIRECTION ( 'NONE',  ( -0.000000000000000000, -1.000000000000000000, -0.000000000000000000 ) ) ;
#10520 = ORIENTED_EDGE ( 'NONE', *, *, #1803, .F. ) ;
#10521 = COLOUR_RGB ( '',1.000000000000000000, 0.9490196078431372140, 0.9098039215686274384 ) ;
#10522 = CARTESIAN_POINT ( 'NONE',  ( 2.299999999999989608, 90.00000000000000000, 8.000000000000000000 ) ) ;
#10523 = DIRECTION ( 'NONE',  ( -1.000000000000000000, 0.000000000000000000, -0.000000000000000000 ) ) ;
#10524 = CARTESIAN_POINT ( 'NONE',  ( 3.033375984251971413, -3.035766082959412415E-15, 0.000000000000000000 ) ) ;
#10525 = VERTEX_POINT ( 'NONE', #8020 ) ;
#10526 = CIRCLE ( 'NONE', #2175, 1.000000000000000000 ) ;
#10527 = DIRECTION ( 'NONE',  ( -0.000000000000000000, -0.000000000000000000, -1.000000000000000000 ) ) ;
#10528 = SHAPE_DEFINITION_REPRESENTATION ( #6461, #9937 ) ;
#10529 = CARTESIAN_POINT ( 'NONE',  ( 3.800000000000025135, 71.98667160128366049, 4.250000001229034652 ) ) ;
#10530 = EDGE_CURVE ( 'NONE', #4697, #7837, #1136, .T. ) ;
#10531 = ORIENTED_EDGE ( 'NONE', *, *, #254, .F. ) ;
#10532 = CARTESIAN_POINT ( 'NONE',  ( 5.000000000000007994, 90.00000000000000000, -3.000000000000000000 ) ) ;
#10533 = VERTEX_POINT ( 'NONE', #8991 ) ;
#10534 = DIRECTION ( 'NONE',  ( -0.8660254037844361541, -0.5000000000000042188, -9.389466242107209433E-17 ) ) ;
#10535 = FACE_OUTER_BOUND ( 'NONE', #11041, .T. ) ;
#10536 = VERTEX_POINT ( 'NONE', #13 ) ;
#10537 = CARTESIAN_POINT ( 'NONE',  ( 3.591865698314129496, 91.49237114305354623, 2.999999999999999556 ) ) ;
#10538 = DIRECTION ( 'NONE',  ( 1.000000000000000000, 0.000000000000000000, -1.445602896647339656E-17 ) ) ;
#10539 = AXIS2_PLACEMENT_3D ( 'NONE', #3634, #10429, #1598 ) ;
#10540 = UNCERTAINTY_MEASURE_WITH_UNIT (LENGTH_MEASURE( 1.000000000000000082E-05 ), #2138, 'distance_accuracy_value', 'NONE');
#10541 = AXIS2_PLACEMENT_3D ( 'NONE', #2728, #7498, #1537 ) ;
#10542 = VERTEX_POINT ( 'NONE', #4164 ) ;
#10543 = CARTESIAN_POINT ( 'NONE',  ( 19.27821517812500574, 117.2309300971526937, 3.434375000614517059 ) ) ;
#10544 = ORIENTED_EDGE ( 'NONE', *, *, #5548, .F. ) ;
#10545 = DIRECTION ( 'NONE',  ( 0.000000000000000000, 0.000000000000000000, 1.000000000000000000 ) ) ;
#10546 = EDGE_CURVE ( 'NONE', #169, #5034, #2923, .T. ) ;
#10547 = VERTEX_POINT ( 'NONE', #7098 ) ;
#10548 = VECTOR ( 'NONE', #2618, 1000.000000000000114 ) ;
#10549 = CARTESIAN_POINT ( 'NONE',  ( 50.72178482187499071, 117.2309300971526937, 2.909375000614517148 ) ) ;
#10550 = ORIENTED_EDGE ( 'NONE', *, *, #4912, .F. ) ;
#10551 = AXIS2_PLACEMENT_3D ( 'NONE', #12458, #1660, #7483 ) ;
#10552 = DIRECTION ( 'NONE',  ( -0.000000000000000000, -1.000000000000000000, -0.000000000000000000 ) ) ;
#10553 = FACE_OUTER_BOUND ( 'NONE', #5817, .T. ) ;
#10554 = DIRECTION ( 'NONE',  ( -0.000000000000000000, 1.000000000000000000, 1.224646799147353207E-16 ) ) ;
#10555 = CARTESIAN_POINT ( 'NONE',  ( 35.00000000000000000, 90.00000000000000000, 22.38477631085024555 ) ) ;
#10556 = EDGE_CURVE ( 'NONE', #6404, #9125, #8151, .T. ) ;
#10557 = CARTESIAN_POINT ( 'NONE',  ( -0.1038759689922479496, -3.348389132562988646, -0.8000000000000000444 ) ) ;
#10558 = EDGE_CURVE ( 'NONE', #9996, #11555, #4100, .T. ) ;
#10559 = VECTOR ( 'NONE', #2538, 1000.000000000000227 ) ;
#10560 = DIRECTION ( 'NONE',  ( -0.7071067811865472397, 0.000000000000000000, 0.7071067811865479058 ) ) ;
#10561 = DIRECTION ( 'NONE',  ( -0.000000000000000000, 1.000000000000000000, -0.000000000000000000 ) ) ;
#10562 = CARTESIAN_POINT ( 'NONE',  ( 7.577945032559769700, 99.43561875886716450, 2.000000000000002665 ) ) ;
#10563 = FACE_OUTER_BOUND ( 'NONE', #2601, .T. ) ;
#10564 = ADVANCED_FACE ( 'NONE', ( #82 ), #12139, .T. ) ;
#10565 = CARTESIAN_POINT ( 'NONE',  ( -48.33333333333332860, -5.000000000000000000, -1.734723475976807094E-15 ) ) ;
#10566 = LINE ( 'NONE', #8543, #3777 ) ;
#10567 = VECTOR ( 'NONE', #6244, 1000.000000000000000 ) ;
#10568 = CARTESIAN_POINT ( 'NONE',  ( 34.25000000000000000, 93.41869858279433458, -8.000000000000000000 ) ) ;
#10569 = ORIENTED_EDGE ( 'NONE', *, *, #8751, .F. ) ;
#10570 = CARTESIAN_POINT ( 'NONE',  ( 3.800000000000015365, 90.00000000000000000, 4.549999999999999822 ) ) ;
#10571 = FACE_OUTER_BOUND ( 'NONE', #8955, .T. ) ;
#10572 = ORIENTED_EDGE ( 'NONE', *, *, #8483, .F. ) ;
#10573 = PRESENTATION_STYLE_ASSIGNMENT (( #4425 ) ) ;
#10574 = LINE ( 'NONE', #4555, #12834 ) ;
#10575 = AXIS2_PLACEMENT_3D ( 'NONE', #3507, #10936, #9833 ) ;
#10576 = EDGE_CURVE ( 'NONE', #10533, #6247, #7889, .T. ) ;
#10577 = CARTESIAN_POINT ( 'NONE',  ( 9.999999999999994671, 70.41451884327426569, 3.000000000000000000 ) ) ;
#10578 = VECTOR ( 'NONE', #3525, 1000.000000000000000 ) ;
#10579 = ORIENTED_EDGE ( 'NONE', *, *, #301, .T. ) ;
#10580 = CARTESIAN_POINT ( 'NONE',  ( -43.33333333333332860, 41.93190556325237850, 3.000000000000000000 ) ) ;
#10581 = ORIENTED_EDGE ( 'NONE', *, *, #2406, .F. ) ;
#10582 = LINE ( 'NONE', #4032, #7537 ) ;
#10583 = DIRECTION ( 'NONE',  ( -1.000000000000000000, -0.000000000000000000, -0.000000000000000000 ) ) ;
#10584 = ORIENTED_EDGE ( 'NONE', *, *, #9570, .T. ) ;
#10585 = CARTESIAN_POINT ( 'NONE',  ( -6.666666666666660745, -5.000000000000000000, 0.000000000000000000 ) ) ;
#10586 = EDGE_LOOP ( 'NONE', ( #12349, #4560, #11734, #4299, #12479, #12612 ) ) ;
#10587 = AXIS2_PLACEMENT_3D ( 'NONE', #12532, #11411, #2461 ) ;
#10588 = CARTESIAN_POINT ( 'NONE',  ( 66.19999999999988916, 71.98667160128361786, 3.950000001229034829 ) ) ;
#10589 = DIRECTION ( 'NONE',  ( 0.000000000000000000, 0.000000000000000000, -1.000000000000000000 ) ) ;
#10590 = CARTESIAN_POINT ( 'NONE',  ( -60.00000000000000000, 30.00000000000000000, -2.500000000000000000 ) ) ;
#10591 = EDGE_CURVE ( 'NONE', #1353, #11880, #6046, .T. ) ;
#10592 = LINE ( 'NONE', #636, #5089 ) ;
#10593 =( BOUNDED_SURFACE ( )  B_SPLINE_SURFACE ( 1, 2, ( 
 ( #9699, #3889, #7868, #11857, #4985, #735, #1052, #8260, #62, #7210, #5307, #127, #4334, #6225, #3098, #8131, #1253, #11258, #6154, #9035, #3296, #2047, #4142, #2179, #2313, #5246, #12117, #10217, #4207, #10151, #8323, #12250, #3164, #253, #4077, #5177, #7141, #11198, #3028, #8193, #1185, #10995, #9299, #7275, #7078, #9166, #2251, #1116, #6024, #5045, #190, #11123, #11059, #10020, #7015 ),
 ( #325, #5109, #12181, #8066, #12051, #2113, #9232, #6090, #10079, #3230, #4271, #6288, #10280, #1313, #9103, #7467, #12312, #2632, #6481, #9625, #4398, #6349, #5634, #11452, #8586, #2565, #2504, #5568, #7338, #4529, #11322, #11388, #1380, #586, #4658, #3360, #1511, #8453, #10543, #5497, #10474, #9495, #3420, #6544, #7402, #4592, #10346, #3552, #3618, #5368, #12577, #1578, #7596, #519, #651 ) ),
 .UNSPECIFIED., .F., .F., .F. ) 
 B_SPLINE_SURFACE_WITH_KNOTS ( ( 2, 2 ),
 ( 3, 2, 2, 2, 2, 2, 2, 2, 2, 2, 2, 2, 2, 2, 2, 2, 2, 2, 2, 2, 2, 2, 2, 2, 2, 2, 2, 3 ),
 ( 0.000000000000000000, 1.000000000000000000 ),
 ( 0.000000000000000000, 0.03333333333333333287, 0.06666666666666666574, 0.1000000000000000056, 0.1333333333333333315, 0.1666666666666666574, 0.2000000000000000111, 0.2333333333333333370, 0.2666666666666666630, 0.2999999999999999889, 0.3333333333333333148, 0.3666666666666666408, 0.4000000000000000222, 0.4333333333333333481, 0.4666666666666666741, 0.5000000000000000000, 0.5333333333333333259, 0.5666666666666666519, 0.5999999999999999778, 0.6333333333333333037, 0.6666666666666666297, 0.6999999999999999556, 0.7333333333333332815, 0.7666666666666667185, 0.8000000000000000444, 0.8333333333333333703, 0.8666666666666666963, 0.8887752010443024098 ),
 .UNSPECIFIED. ) 
 GEOMETRIC_REPRESENTATION_ITEM ( )  RATIONAL_B_SPLINE_SURFACE ( (
 ( 1.000000000000000000, 0.8660254037844387076, 1.000000000000000000, 0.8660254037844387076, 1.000000000000000000, 0.8660254037844387076, 1.000000000000000000, 0.8660254037844387076, 1.000000000000000000, 0.8660254037844387076, 1.000000000000000000, 0.8660254037844387076, 1.000000000000000000, 0.8660254037844387076, 1.000000000000000000, 0.8660254037844387076, 1.000000000000000000, 0.8660254037844387076, 1.000000000000000000, 0.8660254037844387076, 1.000000000000000000, 0.8660254037844387076, 1.000000000000000000, 0.8660254037844387076, 1.000000000000000000, 0.8660254037844387076, 1.000000000000000000, 0.8660254037844387076, 1.000000000000000000, 0.8660254037844387076, 1.000000000000000000, 0.8660254037844387076, 1.000000000000000000, 0.8660254037844387076, 1.000000000000000000, 0.8660254037844387076, 1.000000000000000000, 0.8660254037844387076, 1.000000000000000000, 0.8660254037844387076, 1.000000000000000000, 0.8660254037844387076, 1.000000000000000000, 0.8660254037844387076, 1.000000000000000000, 0.8660254037844387076, 1.000000000000000000, 0.8660254037844387076, 1.000000000000000000, 0.8660254037844387076, 1.000000000000000000, 0.8660254037844387076, 1.000000000000000000, 0.9111405410151519613, 0.9401542262549813511),
 ( 1.000000000000000000, 0.8660254037844387076, 1.000000000000000000, 0.8660254037844387076, 1.000000000000000000, 0.8660254037844387076, 1.000000000000000000, 0.8660254037844387076, 1.000000000000000000, 0.8660254037844387076, 1.000000000000000000, 0.8660254037844387076, 1.000000000000000000, 0.8660254037844387076, 1.000000000000000000, 0.8660254037844387076, 1.000000000000000000, 0.8660254037844387076, 1.000000000000000000, 0.8660254037844387076, 1.000000000000000000, 0.8660254037844387076, 1.000000000000000000, 0.8660254037844387076, 1.000000000000000000, 0.8660254037844387076, 1.000000000000000000, 0.8660254037844387076, 1.000000000000000000, 0.8660254037844387076, 1.000000000000000000, 0.8660254037844387076, 1.000000000000000000, 0.8660254037844387076, 1.000000000000000000, 0.8660254037844387076, 1.000000000000000000, 0.8660254037844387076, 1.000000000000000000, 0.8660254037844387076, 1.000000000000000000, 0.8660254037844387076, 1.000000000000000000, 0.8660254037844387076, 1.000000000000000000, 0.8660254037844387076, 1.000000000000000000, 0.8660254037844387076, 1.000000000000000000, 0.8660254037844387076, 1.000000000000000000, 0.8660254037844387076, 1.000000000000000000, 0.9111405410151519613, 0.9401542262549813511) ) ) 
 REPRESENTATION_ITEM ( '' )  SURFACE ( )  );
#10594 = CYLINDRICAL_SURFACE ( 'NONE', #5405, 3.500000000000003109 ) ;
#10595 = ORIENTED_EDGE ( 'NONE', *, *, #12775, .T. ) ;
#10596 = CARTESIAN_POINT ( 'NONE',  ( 8.499999999999992895, 69.54849343948981755, 1.000000000000000000 ) ) ;
#10597 = CARTESIAN_POINT ( 'NONE',  ( 50.60000000000001563, 62.98000740192552627, 3.462500001229034563 ) ) ;
#10598 = VECTOR ( 'NONE', #5541, 1000.000000000000114 ) ;
#10599 = VERTEX_POINT ( 'NONE', #6902 ) ;
#10600 = ORIENTED_EDGE ( 'NONE', *, *, #9094, .F. ) ;
#10601 = EDGE_LOOP ( 'NONE', ( #10223, #2034, #95 ) ) ;
#10602 = CARTESIAN_POINT ( 'NONE',  ( 7.575919367743916943, 99.43635506061835372, 1.000000000000003109 ) ) ;
#10603 = LINE ( 'NONE', #5630, #11456 ) ;
#10604 = ADVANCED_BREP_SHAPE_REPRESENTATION ( '', ( #11875, #5704 ), #258 ) ;
#10605 = ADVANCED_FACE ( 'NONE', ( #10890 ), #9975, .T. ) ;
#10606 = VECTOR ( 'NONE', #6504, 1000.000000000000000 ) ;
#10607 = EDGE_CURVE ( 'NONE', #2423, #8376, #11345, .T. ) ;
#10608 = ORIENTED_EDGE ( 'NONE', *, *, #1687, .F. ) ;
#10609 = CARTESIAN_POINT ( 'NONE',  ( 3.800000000000039790, 71.98667160128364628, 4.250000001229034652 ) ) ;
#10610 = ORIENTED_EDGE ( 'NONE', *, *, #2406, .T. ) ;
#10611 = LINE ( 'NONE', #10415, #2917 ) ;
#10612 = EDGE_LOOP ( 'NONE', ( #8713, #5399, #10387, #5178 ) ) ;
#10613 = CARTESIAN_POINT ( 'NONE',  ( 35.00000000000000711, 53.69209320379640360, 3.171875000614517326 ) ) ;
#10614 = ORIENTED_EDGE ( 'NONE', *, *, #9680, .F. ) ;
#10615 = CIRCLE ( 'NONE', #8932, 1.599999999999997202 ) ;
#10616 = DIRECTION ( 'NONE',  ( -1.000000000000000000, 0.000000000000000000, 0.000000000000000000 ) ) ;
#10617 = CARTESIAN_POINT ( 'NONE',  ( 20.00000000000000355, 2.000000000000000000, 1.499999999999999556 ) ) ;
#10618 = DIRECTION ( 'NONE',  ( -0.4999999999999987232, 0.8660254037844393737, 0.000000000000000000 ) ) ;
#10619 = EDGE_CURVE ( 'NONE', #7663, #619, #3818, .T. ) ;
#10620 = FACE_BOUND ( 'NONE', #5414, .T. ) ;
#10621 = AXIS2_PLACEMENT_3D ( 'NONE', #4952, #6910, #10960 ) ;
#10622 = CARTESIAN_POINT ( 'NONE',  ( 40.00000000000000000, 0.000000000000000000, 1.500000000000001332 ) ) ;
#10623 = DIRECTION ( 'NONE',  ( 0.000000000000000000, 0.000000000000000000, 1.000000000000000000 ) ) ;
#10624 = DIRECTION ( 'NONE',  ( -1.000000000000000000, 0.000000000000000000, 0.000000000000000000 ) ) ;
#10625 = CARTESIAN_POINT ( 'NONE',  ( 5.000000000000004441, 27.00000000000000000, 2.500000000000000444 ) ) ;
#10626 = ADVANCED_FACE ( 'NONE', ( #3316 ), #11410, .F. ) ;
#10627 = DIRECTION ( 'NONE',  ( -0.5000000000000042188, 1.060575238724903710E-16, -0.8660254037844361541 ) ) ;
#10628 = CARTESIAN_POINT ( 'NONE',  ( 66.20000000000004547, 108.0133283987162969, 3.575000001229034385 ) ) ;
#10629 = ORIENTED_EDGE ( 'NONE', *, *, #8366, .F. ) ;
#10630 =( NAMED_UNIT ( * ) SI_UNIT ( $, .STERADIAN. ) SOLID_ANGLE_UNIT ( ) );
#10631 = CARTESIAN_POINT ( 'NONE',  ( 0.000000000000000000, 0.000000000000000000, -10.00000000000000000 ) ) ;
#10632 = VERTEX_POINT ( 'NONE', #3445 ) ;
#10633 = DIRECTION ( 'NONE',  ( 0.5000000000000036637, -0.8660254037844365982, 0.000000000000000000 ) ) ;
#10634 = DIRECTION ( 'NONE',  ( -0.8660254037844400399, 0.000000000000000000, -0.4999999999999975575 ) ) ;
#10635 = ORIENTED_EDGE ( 'NONE', *, *, #11013, .T. ) ;
#10636 = LINE ( 'NONE', #2667, #9919 ) ;
#10637 = EDGE_CURVE ( 'NONE', #8179, #5076, #2734, .T. ) ;
#10638 = CARTESIAN_POINT ( 'NONE',  ( 66.44356964374999563, 90.00000000000000000, 3.228125000614517237 ) ) ;
#10639 = EDGE_CURVE ( 'NONE', #7985, #485, #6308, .T. ) ;
#10640 = CARTESIAN_POINT ( 'NONE',  ( 35.00000000000000000, 90.00000000000000000, 22.38477631085024555 ) ) ;
#10641 = DIRECTION ( 'NONE',  ( 0.000000000000000000, 0.000000000000000000, -1.000000000000000000 ) ) ;
#10642 = ORIENTED_EDGE ( 'NONE', *, *, #5242, .F. ) ;
#10643 = AXIS2_PLACEMENT_3D ( 'NONE', #5370, #2443, #1513 ) ;
#10644 = DIRECTION ( 'NONE',  ( -0.000000000000000000, 1.000000000000000000, -0.000000000000000000 ) ) ;
#10645 = VERTEX_POINT ( 'NONE', #6245 ) ;
#10646 = FACE_OUTER_BOUND ( 'NONE', #3668, .T. ) ;
#10647 = LINE ( 'NONE', #1624, #5818 ) ;
#10648 = CARTESIAN_POINT ( 'NONE',  ( 66.19999999999998863, 90.00000000000000000, 3.987500001229034030 ) ) ;
#10649 = VERTEX_POINT ( 'NONE', #7423 ) ;
#10651 = DIRECTION ( 'NONE',  ( -1.000000000000000000, 0.000000000000000000, -0.000000000000000000 ) ) ;
#10650 = AXIS2_PLACEMENT_3D ( 'NONE', #9135, #226, #11950 ) ;
#10652 = VERTEX_POINT ( 'NONE', #7234 ) ;
#10653 = CARTESIAN_POINT ( 'NONE',  ( -60.00000000000000000, -6.000000000000000000, 14.99999999999999645 ) ) ;
#10654 = ITEM_DEFINED_TRANSFORMATION ( 'NONE', 'NONE', #12404,  #5704 ) ;
#10655 = CARTESIAN_POINT ( 'NONE',  ( 21.49999999999998579, 90.00000000000000000, -8.000000000000000000 ) ) ;
#10656 = ORIENTED_EDGE ( 'NONE', *, *, #2248, .F. ) ;
#10657 = LINE ( 'NONE', #1760, #3265 ) ;
#10658 = ORIENTED_EDGE ( 'NONE', *, *, #8811, .F. ) ;
#10659 = DIRECTION ( 'NONE',  ( 0.000000000000000000, 0.000000000000000000, 1.000000000000000000 ) ) ;
#10660 = ORIENTED_EDGE ( 'NONE', *, *, #12311, .T. ) ;
#10661 = EDGE_CURVE ( 'NONE', #3461, #1892, #11281, .T. ) ;
#10662 = FACE_OUTER_BOUND ( 'NONE', #5201, .T. ) ;
#10663 = VECTOR ( 'NONE', #11878, 1000.000000000000000 ) ;
#10664 = DIRECTION ( 'NONE',  ( -0.000000000000000000, -0.000000000000000000, -1.000000000000000000 ) ) ;
#10665 = CIRCLE ( 'NONE', #11711, 31.19999999999998863 ) ;
#10666 =( BOUNDED_CURVE ( )  B_SPLINE_CURVE ( 2, ( #1242, #7196, #12103, #8055, #3151, #10010, #2164 ),
 .UNSPECIFIED., .F., .T. ) 
 B_SPLINE_CURVE_WITH_KNOTS ( ( 3, 2, 2, 3 ),
 ( 0.5000000000000001110, 0.5333333333333334370, 0.5666666666666666519, 0.5999999999999999778 ),
 .UNSPECIFIED. ) 
 CURVE ( )  GEOMETRIC_REPRESENTATION_ITEM ( )  RATIONAL_B_SPLINE_CURVE ( ( 0.9999999999999995559, 0.8660254037844391517, 1.000000000000000000, 0.8660254037844387076, 1.000000000000000000, 0.8660254037844387076, 1.000000000000000000 ) ) 
 REPRESENTATION_ITEM ( '' )  );
#10667 = ORIENTED_EDGE ( 'NONE', *, *, #7973, .T. ) ;
#10668 = FACE_OUTER_BOUND ( 'NONE', #5829, .T. ) ;
#10669 = ORIENTED_EDGE ( 'NONE', *, *, #10438, .F. ) ;
#10670 = FACE_OUTER_BOUND ( 'NONE', #1300, .T. ) ;
#10671 = ORIENTED_EDGE ( 'NONE', *, *, #725, .F. ) ;
#10672 = VECTOR ( 'NONE', #3172, 1000.000000000000000 ) ;
#10673 = EDGE_CURVE ( 'NONE', #9073, #6886, #9621, .T. ) ;
#10674 = CARTESIAN_POINT ( 'NONE',  ( 50.72178482187499071, 117.2309300971526937, 3.303125000614517415 ) ) ;
#10675 = EDGE_LOOP ( 'NONE', ( #1011, #10877, #11201, #12854 ) ) ;
#10676 = EDGE_CURVE ( 'NONE', #10005, #12318, #11216, .T. ) ;
#10677 = LINE ( 'NONE', #8528, #3798 ) ;
#10678 = CARTESIAN_POINT ( 'NONE',  ( 31.59522469073172601, 84.46307801270442894, 4.000000000000000000 ) ) ;
#10679 = EDGE_CURVE ( 'NONE', #9678, #3833, #5386, .T. ) ;
#10680 = SURFACE_STYLE_FILL_AREA ( #5577 ) ;
#10681 = CARTESIAN_POINT ( 'NONE',  ( 35.00000000000000000, 126.0266567974326222, 4.100000001229034297 ) ) ;
#10682 = AXIS2_PLACEMENT_3D ( 'NONE', #12830, #5100, #50 ) ;
#10683 = DIRECTION ( 'NONE',  ( -1.000000000000000000, -0.000000000000000000, -0.000000000000000000 ) ) ;
#10684 = CARTESIAN_POINT ( 'NONE',  ( 1.040000000000000036, -0.8660254037844385966, -0.4999999999999997780 ) ) ;
#10685 = LINE ( 'NONE', #8539, #12096 ) ;
#10686 = CARTESIAN_POINT ( 'NONE',  ( 20.90786924106107847, 118.1001848103160512, 2.999999999999999112 ) ) ;
#10687 = DIRECTION ( 'NONE',  ( -1.000000000000000000, 0.000000000000000000, 0.000000000000000000 ) ) ;
#10688 = EDGE_CURVE ( 'NONE', #4963, #655, #2460, .T. ) ;
#10689 = CARTESIAN_POINT ( 'NONE',  ( 20.00000000000000355, 62.64236852357281293, -1.499999999999999556 ) ) ;
#10690 = CARTESIAN_POINT ( 'NONE',  ( 66.44356964374999563, 71.84604660189820891, 3.246875000614517059 ) ) ;
#10691 = ORIENTED_EDGE ( 'NONE', *, *, #3674, .F. ) ;
#10692 = CARTESIAN_POINT ( 'NONE',  ( 35.00000000000000000, 126.0266567974326222, 3.087499999999999911 ) ) ;
#10693 = DIRECTION ( 'NONE',  ( -0.000000000000000000, 0.000000000000000000, -1.000000000000000000 ) ) ;
#10694 = EDGE_LOOP ( 'NONE', ( #1091, #9346, #6436, #11972, #246 ) ) ;
#10695 = VECTOR ( 'NONE', #674, 1000.000000000000000 ) ;
#10696 = CARTESIAN_POINT ( 'NONE',  ( 66.19999999999998863, 90.00000000000000000, 4.325000000000000178 ) ) ;
#10697 = DIRECTION ( 'NONE',  ( -0.000000000000000000, -0.000000000000000000, -1.000000000000000000 ) ) ;
#10698 = LINE ( 'NONE', #7694, #5948 ) ;
#10699 = CARTESIAN_POINT ( 'NONE',  ( 9.999999999999994671, 30.00000000000000000, -2.500000000000000000 ) ) ;
#10700 = EDGE_CURVE ( 'NONE', #9191, #2419, #6057, .T. ) ;
#10701 = LINE ( 'NONE', #8867, #8372 ) ;
#10702 = CARTESIAN_POINT ( 'NONE',  ( 3.556430356250014579, 108.1539533981018053, 4.371875000614516615 ) ) ;
#10703 = ORIENTED_EDGE ( 'NONE', *, *, #12475, .F. ) ;
#10704 = AXIS2_PLACEMENT_3D ( 'NONE', #7895, #12931, #2869 ) ;
#10705 = DIRECTION ( 'NONE',  ( 0.000000000000000000, 0.000000000000000000, 1.000000000000000000 ) ) ;
#10706 = VERTEX_POINT ( 'NONE', #4419 ) ;
#10707 = DIRECTION ( 'NONE',  ( -1.000000000000000000, 0.000000000000000000, 0.000000000000000000 ) ) ;
#10708 = DIRECTION ( 'NONE',  ( -1.000000000000000000, 0.000000000000000000, 0.000000000000000000 ) ) ;
#10709 = EDGE_CURVE ( 'NONE', #7921, #10844, #10458, .T. ) ;
#10710 = EDGE_CURVE ( 'NONE', #7786, #6465, #5236, .T. ) ;
#10711 = CARTESIAN_POINT ( 'NONE',  ( 66.20000000000008811, 108.0133283987162542, 4.362499999999998934 ) ) ;
#10712 = DIRECTION ( 'NONE',  ( -0.8660254037844400399, 0.000000000000000000, -0.4999999999999975575 ) ) ;
#10713 = DIRECTION ( 'NONE',  ( 0.000000000000000000, -1.000000000000000000, 1.370729058197317775E-18 ) ) ;
#10714 = DIRECTION ( 'NONE',  ( -1.000000000000000000, 0.000000000000000000, -0.000000000000000000 ) ) ;
#10715 = ORIENTED_EDGE ( 'NONE', *, *, #10822, .T. ) ;
#10716 = CARTESIAN_POINT ( 'NONE',  ( -18.33333333333332504, 2.000000000000000000, 7.999999999999996447 ) ) ;
#10717 = LINE ( 'NONE', #3859, #11276 ) ;
#10718 = ORIENTED_EDGE ( 'NONE', *, *, #3656, .T. ) ;
#10719 = AXIS2_PLACEMENT_3D ( 'NONE', #848, #2830, #7922 ) ;
#10720 = DIRECTION ( 'NONE',  ( -0.5000000000000042188, 0.000000000000000000, 0.8660254037844361541 ) ) ;
#10721 = ORIENTED_EDGE ( 'NONE', *, *, #3629, .F. ) ;
#10722 = ORIENTED_EDGE ( 'NONE', *, *, #5921, .T. ) ;
#10723 = CARTESIAN_POINT ( 'NONE',  ( 3.759352622210971440, 86.36930750081523911, 3.000000000000000888 ) ) ;
#10724 = CARTESIAN_POINT ( 'NONE',  ( 46.89999999999997016, 90.00000000000000000, -10.00000000000000000 ) ) ;
#10725 = PRODUCT_DEFINITION ( 'UNKNOWN', '', #1762, #4215 ) ;
#10726 = ORIENTED_EDGE ( 'NONE', *, *, #812, .F. ) ;
#10727 = LINE ( 'NONE', #10916, #6161 ) ;
#10728 = ORIENTED_EDGE ( 'NONE', *, *, #1911, .T. ) ;
#10729 = EDGE_CURVE ( 'NONE', #58, #1701, #2393, .T. ) ;
#10730 = DIRECTION ( 'NONE',  ( 0.000000000000000000, 0.000000000000000000, -1.000000000000000000 ) ) ;
#10731 = AXIS2_PLACEMENT_3D ( 'NONE', #8494, #6515, #6451 ) ;
#10732 = ORIENTED_EDGE ( 'NONE', *, *, #517, .F. ) ;
#10733 = CARTESIAN_POINT ( 'NONE',  ( 38.50000000000000711, 90.00000000000000000, 6.000000000000000000 ) ) ;
#10734 = ORIENTED_EDGE ( 'NONE', *, *, #705, .T. ) ;
#10735 = DIRECTION ( 'NONE',  ( -1.000000000000000000, 0.000000000000000000, 0.000000000000000000 ) ) ;
#10736 = AXIS2_PLACEMENT_3D ( 'NONE', #6510, #7564, #5397 ) ;
#10737 = DIRECTION ( 'NONE',  ( 0.000000000000000000, 0.000000000000000000, 1.000000000000000000 ) ) ;
#10738 = VECTOR ( 'NONE', #6508, 1000.000000000000000 ) ;
#10739 = FILL_AREA_STYLE ('',( #729 ) ) ;
#10740 = CARTESIAN_POINT ( 'NONE',  ( 35.00000000000000000, 126.3079067962035822, 3.790625000614517237 ) ) ;
#10741 = EDGE_CURVE ( 'NONE', #294, #408, #4817, .T. ) ;
#10742 = CARTESIAN_POINT ( 'NONE',  ( -61.00000000000000711, 31.73205080756887142, 3.000000000000000000 ) ) ;
#10743 = CARTESIAN_POINT ( 'NONE',  ( 35.00000000000000711, 53.97334320256736362, 4.325000001229033941 ) ) ;
#10744 = DIRECTION ( 'NONE',  ( 0.000000000000000000, 0.000000000000000000, 1.000000000000000000 ) ) ;
#10745 = VECTOR ( 'NONE', #5854, 1000.000000000000000 ) ;
#10746 = EDGE_CURVE ( 'NONE', #9892, #7985, #12270, .T. ) ;
#10747 = LINE ( 'NONE', #8973, #12306 ) ;
#10748 = CARTESIAN_POINT ( 'NONE',  ( 29.40717483660827014, 120.9786552847847361, 2.999999999999999112 ) ) ;
#10749 = VECTOR ( 'NONE', #6105, 1000.000000000000000 ) ;
#10750 = CARTESIAN_POINT ( 'NONE',  ( 64.54728993811707483, 100.7543353701752125, 2.858851390224067313 ) ) ;
#10751 = DIRECTION ( 'NONE',  ( 0.000000000000000000, -0.000000000000000000, -1.000000000000000000 ) ) ;
#10752 = CARTESIAN_POINT ( 'NONE',  ( 50.72178482187501203, 62.76906990284730625, 4.559375000614517504 ) ) ;
#10753 = ORIENTED_EDGE ( 'NONE', *, *, #168, .F. ) ;
#10754 = CARTESIAN_POINT ( 'NONE',  ( 50.60000000000001563, 62.98000740192552627, 4.700000000000000178 ) ) ;
#10755 = DIRECTION ( 'NONE',  ( 0.000000000000000000, 0.000000000000000000, 1.000000000000000000 ) ) ;
#10756 = ORIENTED_EDGE ( 'NONE', *, *, #12549, .T. ) ;
#10757 = VECTOR ( 'NONE', #6916, 1000.000000000000227 ) ;
#10758 = PRODUCT_DEFINITION_SHAPE ( 'NONE', 'NONE',  #12966 ) ;
#10759 =( NAMED_UNIT ( * ) PLANE_ANGLE_UNIT ( ) SI_UNIT ( $, .RADIAN. ) );
#10760 = AXIS2_PLACEMENT_3D ( 'NONE', #4609, #9511, #6429 ) ;
#10761 = EDGE_CURVE ( 'NONE', #3535, #10795, #1333, .T. ) ;
#10762 = CARTESIAN_POINT ( 'NONE',  ( 34.25000000000000000, 93.26496554346289258, 4.800000000000000711 ) ) ;
#10763 = DIRECTION ( 'NONE',  ( 0.000000000000000000, -1.000000000000000000, 0.000000000000000000 ) ) ;
#10764 = VECTOR ( 'NONE', #12735, 1000.000000000000000 ) ;
#10765 = DIRECTION ( 'NONE',  ( -0.000000000000000000, 1.000000000000000000, -0.000000000000000000 ) ) ;
#10766 = CARTESIAN_POINT ( 'NONE',  ( 3.556430356250028790, 71.84604660189818048, 3.940625000614517592 ) ) ;
#10767 = AXIS2_PLACEMENT_3D ( 'NONE', #6998, #1236, #10263 ) ;
#10768 = LINE ( 'NONE', #7633, #2104 ) ;
#10769 = CARTESIAN_POINT ( 'NONE',  ( 3.556430356250014579, 108.1539533981018053, 3.921875000614517326 ) ) ;
#10770 = ORIENTED_EDGE ( 'NONE', *, *, #11229, .F. ) ;
#10771 = FACE_OUTER_BOUND ( 'NONE', #11962, .T. ) ;
#10772 = ORIENTED_EDGE ( 'NONE', *, *, #3965, .F. ) ;
#10773 = FILL_AREA_STYLE ('',( #10895 ) ) ;
#10774 = FACE_BOUND ( 'NONE', #4959, .T. ) ;
#10775 = VECTOR ( 'NONE', #9579, 999.9999999999998863 ) ;
#10776 = EDGE_CURVE ( 'NONE', #4584, #7039, #10566, .T. ) ;
#10777 =( BOUNDED_CURVE ( )  B_SPLINE_CURVE ( 2, ( #9342, #3399, #8235, #10257, #10322, #4314, #7377 ),
 .UNSPECIFIED., .F., .F. ) 
 B_SPLINE_CURVE_WITH_KNOTS ( ( 3, 2, 2, 3 ),
 ( 0.8000000000000002665, 0.8333333333333334814, 0.8666666666666666963, 0.8887752010635167066 ),
 .UNSPECIFIED. ) 
 CURVE ( )  GEOMETRIC_REPRESENTATION_ITEM ( )  RATIONAL_B_SPLINE_CURVE ( ( 0.9999999999999991118, 0.8660254037844395958, 1.000000000000000000, 0.8660254037844387076, 1.000000000000000000, 0.9111405409379251807, 0.9401542263054123438 ) ) 
 REPRESENTATION_ITEM ( '' )  );
#10778 = CARTESIAN_POINT ( 'NONE',  ( -0.9999999999999997780, -4.273461295629625845, -0.8000000000000000444 ) ) ;
#10779 = CARTESIAN_POINT ( 'NONE',  ( 50.00000000000000000, 0.000000000000000000, 1.500000000000001332 ) ) ;
#10780 = CARTESIAN_POINT ( 'NONE',  ( 45.00000000000000000, -5.000000000000000000, 4.249999999999999112 ) ) ;
#10781 = DIRECTION ( 'NONE',  ( 0.000000000000000000, 0.000000000000000000, -1.000000000000000000 ) ) ;
#10782 = ORIENTED_EDGE ( 'NONE', *, *, #3925, .F. ) ;
#10783 = LINE ( 'NONE', #7522, #10125 ) ;
#10784 = DIRECTION ( 'NONE',  ( -0.000000000000000000, -0.000000000000000000, 1.000000000000000000 ) ) ;
#10785 = VERTEX_POINT ( 'NONE', #5653 ) ;
#10786 = CARTESIAN_POINT ( 'NONE',  ( -18.33333333333332504, 30.00000000000000000, 7.999999999999996447 ) ) ;
#10787 = ORIENTED_EDGE ( 'NONE', *, *, #388, .T. ) ;
#10788 = ADVANCED_FACE ( 'NONE', ( #800 ), #12558, .F. ) ;
#10789=STYLED_ITEM('',(#12988),#3386);
#10790 = DIRECTION ( 'NONE',  ( 0.000000000000000000, 0.000000000000000000, -1.000000000000000000 ) ) ;
#10791 = EDGE_LOOP ( 'NONE', ( #4487, #116, #12928, #3960 ) ) ;
#10792 = CARTESIAN_POINT ( 'NONE',  ( 35.00000000000000000, 90.00000000000000000, -1.000000000000000000 ) ) ;
#10793 = DIRECTION ( 'NONE',  ( -1.000000000000000000, 0.000000000000000000, 0.000000000000000000 ) ) ;
#10794 = ADVANCED_FACE ( 'NONE', ( #9645 ), #4206, .F. ) ;
#10795 = VERTEX_POINT ( 'NONE', #1601 ) ;
#10796 = VECTOR ( 'NONE', #4616, 1000.000000000000000 ) ;
#10797 = PLANE ( 'NONE',  #5742 ) ;
#10798 = ORIENTED_EDGE ( 'NONE', *, *, #10438, .T. ) ;
#10799 = DIRECTION ( 'NONE',  ( 1.000000000000000000, -0.000000000000000000, -0.000000000000000000 ) ) ;
#10800 = ORIENTED_EDGE ( 'NONE', *, *, #12372, .F. ) ;
#10801 = CARTESIAN_POINT ( 'NONE',  ( 19.27821517812503060, 62.76906990284727783, 3.528125000614517059 ) ) ;
#10802 = VERTEX_POINT ( 'NONE', #1794 ) ;
#10803 = EDGE_CURVE ( 'NONE', #4584, #12930, #12531, .T. ) ;
#10804 = CARTESIAN_POINT ( 'NONE',  ( 67.70000000000001705, 90.00000000000000000, 3.000000000000000000 ) ) ;
#10805 = DIRECTION ( 'NONE',  ( 0.000000000000000000, 0.000000000000000000, -1.000000000000000000 ) ) ;
#10806 = DIRECTION ( 'NONE',  ( -0.3090169943749500048, 0.9510565162951528650, 0.000000000000000000 ) ) ;
#10807 = CARTESIAN_POINT ( 'NONE',  ( 35.00000000000000711, 53.97334320256736362, 3.875000001229034208 ) ) ;
#10808 = LINE ( 'NONE', #1851, #1445 ) ;
#10809 = CARTESIAN_POINT ( 'NONE',  ( 1.269999999999999796, 2.849999999999999201, 0.000000000000000000 ) ) ;
#10810 = DIRECTION ( 'NONE',  ( -1.000000000000000000, -9.570888143320317860E-16, 0.000000000000000000 ) ) ;
#10811 = CARTESIAN_POINT ( 'NONE',  ( -6.666666666666660745, -5.000000000000000000, 0.000000000000000000 ) ) ;
#10812 = CARTESIAN_POINT ( 'NONE',  ( 8.500000000000000000, 66.25713400046146262, 2.999999999999919620 ) ) ;
#10813 = AXIS2_PLACEMENT_3D ( 'NONE', #8413, #3448, #2529 ) ;
#10814 = DIRECTION ( 'NONE',  ( -0.9510565162951533091, -0.3090169943749480619, 0.000000000000000000 ) ) ;
#10815 = ORIENTED_EDGE ( 'NONE', *, *, #5141, .T. ) ;
#10816 = CARTESIAN_POINT ( 'NONE',  ( -998.3826497308103853, 0.000000000000000000, 0.000000000000000000 ) ) ;
#10817 = CARTESIAN_POINT ( 'NONE',  ( 7.576448291486922670, 99.43666122937791840, 4.000000000000000000 ) ) ;
#10818 = VERTEX_POINT ( 'NONE', #3573 ) ;
#10819 = CARTESIAN_POINT ( 'NONE',  ( 3.800000000000025135, 71.98667160128366049, 3.687500000000000888 ) ) ;
#10820 = CARTESIAN_POINT ( 'NONE',  ( 25.00000000000000355, 2.000000000000001332, 5.750000000000000000 ) ) ;
#10821 = EDGE_LOOP ( 'NONE', ( #1638, #7849, #9685, #5038 ) ) ;
#10822 = EDGE_CURVE ( 'NONE', #11636, #10444, #5520, .T. ) ;
#10823 = VECTOR ( 'NONE', #822, 1000.000000000000000 ) ;
#10824 = AXIS2_PLACEMENT_3D ( 'NONE', #6169, #202, #8206 ) ;
#10825 = DIRECTION ( 'NONE',  ( 0.000000000000000000, 0.000000000000000000, 1.000000000000000000 ) ) ;
#10826 = FACE_OUTER_BOUND ( 'NONE', #5876, .T. ) ;
#10827 = CARTESIAN_POINT ( 'NONE',  ( 35.00000000000000000, 90.00000000000000000, -1.000000000000000000 ) ) ;
#10828 = CARTESIAN_POINT ( 'NONE',  ( 66.44356964375000985, 71.84604660189820891, 4.090625000614517504 ) ) ;
#10829 = VECTOR ( 'NONE', #12417, 1000.000000000000000 ) ;
#10830 = DIRECTION ( 'NONE',  ( -0.7071067811865472397, 8.659560562354937789E-17, -0.7071067811865479058 ) ) ;
#10831 = CARTESIAN_POINT ( 'NONE',  ( 3.556430356250014579, 108.1539533981018053, 4.821875000614516793 ) ) ;
#10832 = VERTEX_POINT ( 'NONE', #10689 ) ;
#10833 = EDGE_CURVE ( 'NONE', #9108, #1636, #7684, .T. ) ;
#10834 = ORIENTED_EDGE ( 'NONE', *, *, #2311, .T. ) ;
#10835 = EDGE_CURVE ( 'NONE', #7668, #9926, #7807, .T. ) ;
#10836 = LINE ( 'NONE', #9853, #10511 ) ;
#10837 = LINE ( 'NONE', #7897, #10414 ) ;
#10838 = LINE ( 'NONE', #12935, #8429 ) ;
#10839 = CYLINDRICAL_SURFACE ( 'NONE', #8229, 1.500000000000001332 ) ;
#10840 = DIRECTION ( 'NONE',  ( -1.000000000000000000, 0.000000000000000000, -0.000000000000000000 ) ) ;
#10841 = ORIENTED_EDGE ( 'NONE', *, *, #10069, .T. ) ;
#10842 = CARTESIAN_POINT ( 'NONE',  ( 7.500000000000000000, 34.99999999999999289, -1.499999999999999556 ) ) ;
#10843 = DIRECTION ( 'NONE',  ( -1.000000000000000000, 0.000000000000000000, 0.000000000000000000 ) ) ;
#10844 = VERTEX_POINT ( 'NONE', #4677 ) ;
#10845 = VECTOR ( 'NONE', #7549, 1000.000000000000227 ) ;
#10846 = LINE ( 'NONE', #7971, #7846 ) ;
#10847 = EDGE_LOOP ( 'NONE', ( #1259, #10834, #8944, #7123, #1900 ) ) ;
#10848 = EDGE_CURVE ( 'NONE', #2423, #10475, #11512, .T. ) ;
#10849 = VECTOR ( 'NONE', #9163, 1000.000000000000000 ) ;
#10850 =( NAMED_UNIT ( * ) PLANE_ANGLE_UNIT ( ) SI_UNIT ( $, .RADIAN. ) );
#10851 = ORIENTED_EDGE ( 'NONE', *, *, #516, .T. ) ;
#10852 = DIRECTION ( 'NONE',  ( -5.551115123125781124E-15, 1.000000000000000000, 0.000000000000000000 ) ) ;
#10853 = LINE ( 'NONE', #6732, #2280 ) ;
#10854 = AXIS2_PLACEMENT_3D ( 'NONE', #11983, #3891, #3030 ) ;
#10855 = ORIENTED_EDGE ( 'NONE', *, *, #7521, .T. ) ;
#10856 = DIRECTION ( 'NONE',  ( 0.000000000000000000, 0.000000000000000000, 1.000000000000000000 ) ) ;
#10857 = VERTEX_POINT ( 'NONE', #11540 ) ;
#10858 = LINE ( 'NONE', #12894, #5415 ) ;
#10859 = ORIENTED_EDGE ( 'NONE', *, *, #11997, .T. ) ;
#10860 = CARTESIAN_POINT ( 'NONE',  ( 60.63303222545420823, 111.5086687406912347, 2.829484441871016109 ) ) ;
#10861 = VERTEX_POINT ( 'NONE', #9515 ) ;
#10862 = EDGE_CURVE ( 'NONE', #7972, #2347, #3763, .T. ) ;
#10863 = VECTOR ( 'NONE', #357, 1000.000000000000000 ) ;
#10864 = CARTESIAN_POINT ( 'NONE',  ( 25.00000000000000355, 2.000000000000001332, -5.750000000000000000 ) ) ;
#10865 = LINE ( 'NONE', #8904, #1191 ) ;
#10866 = CARTESIAN_POINT ( 'NONE',  ( 3.556430356250028790, 71.84604660189818048, 3.040625000614517237 ) ) ;
#10867 = DIRECTION ( 'NONE',  ( -0.000000000000000000, 1.000000000000000000, -0.000000000000000000 ) ) ;
#10868 = EDGE_CURVE ( 'NONE', #6711, #10525, #3343, .T. ) ;
#10870 = EDGE_CURVE ( 'NONE', #9344, #5354, #5717, .T. ) ;
#10869 = ORIENTED_EDGE ( 'NONE', *, *, #3010, .F. ) ;
#10871 = AXIS2_PLACEMENT_3D ( 'NONE', #8281, #11474, #10494 ) ;
#10872 = DIRECTION ( 'NONE',  ( 0.000000000000000000, 0.000000000000000000, 1.000000000000000000 ) ) ;
#10873 = LINE ( 'NONE', #1917, #1663 ) ;
#10874 = CARTESIAN_POINT ( 'NONE',  ( 14.01316722111233481, 113.4202627883618248, 3.000000000000000444 ) ) ;
#10875 = ORIENTED_EDGE ( 'NONE', *, *, #11995, .F. ) ;
#10876 = DIRECTION ( 'NONE',  ( -1.000000000000000000, 1.387778780781446938E-14, 0.000000000000000000 ) ) ;
#10877 = ORIENTED_EDGE ( 'NONE', *, *, #6150, .F. ) ;
#10878 = DIRECTION ( 'NONE',  ( 0.000000000000000000, 1.000000000000000000, 0.000000000000000000 ) ) ;
#10879 = CARTESIAN_POINT ( 'NONE',  ( 3.556430356250014579, 108.1539533981018053, 3.471875000614516704 ) ) ;
#10880 = ORIENTED_EDGE ( 'NONE', *, *, #8124, .F. ) ;
#10881 = CARTESIAN_POINT ( 'NONE',  ( 19.27821517812500574, 117.2309300971526937, 4.334375000614516971 ) ) ;
#10882 = CIRCLE ( 'NONE', #2742, 6.499999999999999112 ) ;
#10883 = DIRECTION ( 'NONE',  ( -0.01745240511413415074, -0.9998476951794869061, 0.000000000000000000 ) ) ;
#10884 = CARTESIAN_POINT ( 'NONE',  ( 1.040000000000000036, 0.5773502691896262862, -1.000000000000000000 ) ) ;
#10885 = PRODUCT_RELATED_PRODUCT_CATEGORY ( 'part', '', ( #5313 ) ) ;
#10886 = CARTESIAN_POINT ( 'NONE',  ( 34.25000000000000000, 92.49999999999998579, -8.000000000000000000 ) ) ;
#10887 = VECTOR ( 'NONE', #1907, 1000.000000000000000 ) ;
#10888 = DIRECTION ( 'NONE',  ( -1.000000000000000000, 0.000000000000000000, 0.000000000000000000 ) ) ;
#10889 = EDGE_CURVE ( 'NONE', #9045, #4210, #417, .T. ) ;
#10890 = FACE_OUTER_BOUND ( 'NONE', #5176, .T. ) ;
#10891 = CARTESIAN_POINT ( 'NONE',  ( 35.00000000000000711, 53.69209320379639649, 4.071875000614516793 ) ) ;
#10892 = ORIENTED_EDGE ( 'NONE', *, *, #10987, .F. ) ;
#10893 = DIRECTION ( 'NONE',  ( -1.000000000000000000, 0.000000000000000000, -0.000000000000000000 ) ) ;
#10894 = ORIENTED_EDGE ( 'NONE', *, *, #8822, .T. ) ;
#10895 = FILL_AREA_STYLE_COLOUR ( '', #40 ) ;
#10896 = CARTESIAN_POINT ( 'NONE',  ( 3.800000000000015365, 90.00000000000000000, 4.662500001229034297 ) ) ;
#10898 = EDGE_CURVE ( 'NONE', #4053, #7376, #2656, .T. ) ;
#10897 = LINE ( 'NONE', #8937, #11978 ) ;
#10899 = CARTESIAN_POINT ( 'NONE',  ( -23.49999999999999289, 79.07477288111861924, -1.000000000000000000 ) ) ;
#10900 = CARTESIAN_POINT ( 'NONE',  ( -43.33333333333332860, 39.62250448649387380, 0.9999999999999997780 ) ) ;
#10901 = EDGE_LOOP ( 'NONE', ( #8302, #7176, #2975, #4519, #7636 ) ) ;
#10902 = DIRECTION ( 'NONE',  ( 0.000000000000000000, 0.000000000000000000, 1.000000000000000000 ) ) ;
#10903 = EDGE_CURVE ( 'NONE', #11115, #10542, #9704, .T. ) ;
#10904 = FACE_OUTER_BOUND ( 'NONE', #9101, .T. ) ;
#10905 = VERTEX_POINT ( 'NONE', #6693 ) ;
#10906 = MECHANICAL_DESIGN_GEOMETRIC_PRESENTATION_REPRESENTATION (  '', ( #1930 ), #6727 ) ;
#10907 = ORIENTED_EDGE ( 'NONE', *, *, #59, .F. ) ;
#10908 = FACE_OUTER_BOUND ( 'NONE', #12696, .T. ) ;
#10909 = ORIENTED_EDGE ( 'NONE', *, *, #2035, .F. ) ;
#10910 = PLANE ( 'NONE',  #6733 ) ;
#10911 = DIRECTION ( 'NONE',  ( -0.000000000000000000, -0.5000000000000003331, -0.8660254037844383745 ) ) ;
#10912 = ORIENTED_EDGE ( 'NONE', *, *, #6683, .T. ) ;
#10913 = CIRCLE ( 'NONE', #9246, 1.599999999999990319 ) ;
#10914 = ADVANCED_FACE ( 'NONE', ( #6759 ), #1666, .T. ) ;
#10915 = ORIENTED_EDGE ( 'NONE', *, *, #7392, .T. ) ;
#10916 = CARTESIAN_POINT ( 'NONE',  ( 7.500000000000000000, 34.99999999999999289, 1.499999999999999556 ) ) ;
#10917 = VERTEX_POINT ( 'NONE', #5781 ) ;
#10918 = CYLINDRICAL_SURFACE ( 'NONE', #5843, 3.500000000000003109 ) ;
#10919 = ORIENTED_EDGE ( 'NONE', *, *, #5911, .F. ) ;
#10920 = CARTESIAN_POINT ( 'NONE',  ( 3.556430356250014579, 108.1539533981018053, 4.315625000614517148 ) ) ;
#10921 = EDGE_LOOP ( 'NONE', ( #7407, #11863 ) ) ;
#10922 = PRESENTATION_LAYER_ASSIGNMENT (  '', '', ( #4253 ) ) ;
#10923 = CARTESIAN_POINT ( 'NONE',  ( 48.49999999999995737, 90.00000000000000000, -8.000000000000000000 ) ) ;
#10924 = CARTESIAN_POINT ( 'NONE',  ( 50.72178482187501203, 62.76906990284730625, 3.153125000614517504 ) ) ;
#10925 = DIRECTION ( 'NONE',  ( 1.000000000000000000, 0.000000000000000000, -0.000000000000000000 ) ) ;
#10926 = CARTESIAN_POINT ( 'NONE',  ( 3.556430356250015024, 90.00000000000000000, 3.453125000614517770 ) ) ;
#10927 = AXIS2_PLACEMENT_3D ( 'NONE', #6214, #7065, #179 ) ;
#10928 = LINE ( 'NONE', #4797, #5835 ) ;
#10929 = EDGE_CURVE ( 'NONE', #1906, #5609, #133, .T. ) ;
#10930 = EDGE_LOOP ( 'NONE', ( #12763, #9369, #9406, #1644 ) ) ;
#10931 = CARTESIAN_POINT ( 'NONE',  ( 6.500000000000002665, 68.39379290111055809, 0.9999999999999997780 ) ) ;
#10932 = DIRECTION ( 'NONE',  ( 0.000000000000000000, 0.000000000000000000, 1.000000000000000000 ) ) ;
#10933 = CARTESIAN_POINT ( 'NONE',  ( 7.650000000000000355, 0.000000000000000000, 0.000000000000000000 ) ) ;
#10934 = ORIENTED_EDGE ( 'NONE', *, *, #5436, .T. ) ;
#10935 = AXIS2_PLACEMENT_3D ( 'NONE', #2994, #9920, #826 ) ;
#10936 = DIRECTION ( 'NONE',  ( -5.624500927088228034E-17, 1.370729058197317968E-18, 1.000000000000000000 ) ) ;
#10937 = ORIENTED_EDGE ( 'NONE', *, *, #6127, .F. ) ;
#10938 = LINE ( 'NONE', #9965, #5862 ) ;
#10939 = CARTESIAN_POINT ( 'NONE',  ( 35.00000000000000000, 126.3079067962035822, 4.296875000614517326 ) ) ;
#10941 = EDGE_CURVE ( 'NONE', #7451, #11441, #9419, .T. ) ;
#10940 = ORIENTED_EDGE ( 'NONE', *, *, #5856, .F. ) ;
#10942 = EDGE_CURVE ( 'NONE', #11004, #4871, #7749, .T. ) ;
#10943 = CARTESIAN_POINT ( 'NONE',  ( 3.556430356250015024, 90.00000000000000000, 3.059375000614517059 ) ) ;
#10944 = DIRECTION ( 'NONE',  ( -0.000000000000000000, 1.000000000000000000, -0.000000000000000000 ) ) ;
#10945 = AXIS2_PLACEMENT_3D ( 'NONE', #10038, #6303, #1069 ) ;
#10946 = CONICAL_SURFACE ( 'NONE', #714, 1.499999999999999556, 1.029744260000000189 ) ;
#10947 = CARTESIAN_POINT ( 'NONE',  ( 1.040000000000000036, 0.5773502691896262862, 1.000000000000000000 ) ) ;
#10948 = EDGE_CURVE ( 'NONE', #6839, #10173, #1990, .T. ) ;
#10949 = DIRECTION ( 'NONE',  ( 0.000000000000000000, 0.000000000000000000, 1.000000000000000000 ) ) ;
#10950 = CARTESIAN_POINT ( 'NONE',  ( 35.00000000000000000, 90.00000000000000000, -5.000000000000000000 ) ) ;
#10951 = CARTESIAN_POINT ( 'NONE',  ( -64.48205080756885366, 31.76313972081441150, 1.836970198721030427E-16 ) ) ;
#10952 = VECTOR ( 'NONE', #668, 1000.000000000000000 ) ;
#10953 = DIRECTION ( 'NONE',  ( -0.000000000000000000, 1.000000000000000000, -0.000000000000000000 ) ) ;
#10954 = EDGE_LOOP ( 'NONE', ( #10629, #12301, #6183, #4437 ) ) ;
#10955 = CIRCLE ( 'NONE', #9713, 1.599999999999986766 ) ;
#10956 = CARTESIAN_POINT ( 'NONE',  ( 31.99902028769960438, 88.51116798584881451, -3.000000000000000000 ) ) ;
#10957 = ORIENTED_EDGE ( 'NONE', *, *, #4353, .F. ) ;
#10958 = DIRECTION ( 'NONE',  ( -0.5000000000000043299, 0.8660254037844362651, 0.000000000000000000 ) ) ;
#10959 = EDGE_CURVE ( 'NONE', #3461, #2471, #3036, .T. ) ;
#10960 = DIRECTION ( 'NONE',  ( 0.000000000000000000, -0.5000000000000000000, -0.8660254037844385966 ) ) ;
#10961 = DIRECTION ( 'NONE',  ( 1.000000000000000000, 0.000000000000000000, 0.000000000000000000 ) ) ;
#10962 = AXIS2_PLACEMENT_3D ( 'NONE', #4894, #8034, #8883 ) ;
#10963 = LINE ( 'NONE', #10780, #11986 ) ;
#10964 = AXIS2_PLACEMENT_3D ( 'NONE', #1496, #3346, #2424 ) ;
#10965 = ORIENTED_EDGE ( 'NONE', *, *, #3285, .F. ) ;
#10966 = CARTESIAN_POINT ( 'NONE',  ( 52.49999999999996447, 94.00000000000000000, -10.00000000000000000 ) ) ;
#10967 = CARTESIAN_POINT ( 'NONE',  ( 35.00000000000000000, 126.0266567974326222, 4.100000001229034297 ) ) ;
#10968 = ORIENTED_EDGE ( 'NONE', *, *, #12211, .F. ) ;
#10969 = ORIENTED_EDGE ( 'NONE', *, *, #4361, .F. ) ;
#10970 = FACE_OUTER_BOUND ( 'NONE', #2253, .T. ) ;
#10972 = EDGE_LOOP ( 'NONE', ( #4117, #10937, #775 ) ) ;
#10971 = AXIS2_PLACEMENT_3D ( 'NONE', #9973, #10765, #5980 ) ;
#10973 =( GEOMETRIC_REPRESENTATION_CONTEXT ( 3 ) GLOBAL_UNCERTAINTY_ASSIGNED_CONTEXT ( ( #1082 ) ) GLOBAL_UNIT_ASSIGNED_CONTEXT ( ( #4451, #6470, #3733 ) ) REPRESENTATION_CONTEXT ( 'NONE', 'WORKASPACE' ) );
#10974 = DIRECTION ( 'NONE',  ( 0.3090169943749492276, -0.9510565162951530871, 0.000000000000000000 ) ) ;
#10975 = CARTESIAN_POINT ( 'NONE',  ( 34.25000000000000000, 93.41869858279433458, 6.000000000000000000 ) ) ;
#10976 = ADVANCED_FACE ( 'NONE', ( #7877 ), #5117, .F. ) ;
#10977 = VERTEX_POINT ( 'NONE', #12913 ) ;
#10978 = ORIENTED_EDGE ( 'NONE', *, *, #168, .T. ) ;
#10979 = PLANE ( 'NONE',  #12018 ) ;
#10980 = ORIENTED_EDGE ( 'NONE', *, *, #12332, .T. ) ;
#10981 = CARTESIAN_POINT ( 'NONE',  ( 3.556430356250014579, 108.1539533981018053, 4.315625000614517148 ) ) ;
#10982 =( GEOMETRIC_REPRESENTATION_CONTEXT ( 3 ) GLOBAL_UNCERTAINTY_ASSIGNED_CONTEXT ( ( #11159 ) ) GLOBAL_UNIT_ASSIGNED_CONTEXT ( ( #11955, #3796, #11767 ) ) REPRESENTATION_CONTEXT ( 'NONE', 'WORKASPACE' ) );
#10983 = ORIENTED_EDGE ( 'NONE', *, *, #4213, .T. ) ;
#10984 = ORIENTED_EDGE ( 'NONE', *, *, #9726, .F. ) ;
#10985 = CARTESIAN_POINT ( 'NONE',  ( 62.73303611935715196, 98.48533184915085315, 4.000000000000000000 ) ) ;
#10986 = CARTESIAN_POINT ( 'NONE',  ( 50.72178482187499071, 117.2309300971526937, 3.303125000614517415 ) ) ;
#10987 = EDGE_CURVE ( 'NONE', #2471, #11510, #3958, .T. ) ;
#10988 = PRESENTATION_STYLE_ASSIGNMENT (( #9694 ) ) ;
#10989 = DIRECTION ( 'NONE',  ( -0.3262398754384820410, 0.9452870165584015272, 0.000000000000000000 ) ) ;
#10990 = EDGE_CURVE ( 'NONE', #4210, #9471, #2120, .T. ) ;
#10991 = FILL_AREA_STYLE_COLOUR ( '', #9266 ) ;
#10992 = AXIS2_PLACEMENT_3D ( 'NONE', #8398, #12381, #12450 ) ;
#10993 = CARTESIAN_POINT ( 'NONE',  ( 3.800000000000015365, 90.00000000000000000, 4.100000000000000533 ) ) ;
#10994 = ORIENTED_EDGE ( 'NONE', *, *, #10158, .F. ) ;
#10995 = CARTESIAN_POINT ( 'NONE',  ( 66.19999999999997442, 108.0133283987163253, 3.462499999999999911 ) ) ;
#10996 = CARTESIAN_POINT ( 'NONE',  ( 35.00000000000000000, 90.00000000000000000, 4.000000000000000000 ) ) ;
#10997 = LINE ( 'NONE', #11063, #2829 ) ;
#10998 = ORIENTED_EDGE ( 'NONE', *, *, #10903, .T. ) ;
#10999 = DIRECTION ( 'NONE',  ( -1.000000000000000000, -0.000000000000000000, -0.000000000000000000 ) ) ;
#11000 = EDGE_LOOP ( 'NONE', ( #11589, #10126, #8094, #9362 ) ) ;
#11001 = VECTOR ( 'NONE', #7959, 1000.000000000000114 ) ;
#11002 = DIRECTION ( 'NONE',  ( 0.000000000000000000, 0.000000000000000000, -1.000000000000000000 ) ) ;
#11003 = CARTESIAN_POINT ( 'NONE',  ( 35.00000000000000000, 126.3079067962035822, 4.240625000614517859 ) ) ;
#11004 = VERTEX_POINT ( 'NONE', #10086 ) ;
#11005 = ADVANCED_FACE ( 'NONE', ( #5967 ), #928, .T. ) ;
#11006 = CARTESIAN_POINT ( 'NONE',  ( 35.00000000000000000, 126.3079067962035822, 3.396875000614517415 ) ) ;
#11007 = DIRECTION ( 'NONE',  ( 0.8660254037844361541, 0.5000000000000042188, 0.000000000000000000 ) ) ;
#11008 = PLANE ( 'NONE',  #165 ) ;
#11009 = EDGE_CURVE ( 'NONE', #4788, #3097, #3105, .T. ) ;
#11010 = CIRCLE ( 'NONE', #3515, 3.350000000000003642 ) ;
#11011 = CARTESIAN_POINT ( 'NONE',  ( 7.500000000000000000, 30.00000000000000000, 0.000000000000000000 ) ) ;
#11012 = CARTESIAN_POINT ( 'NONE',  ( 41.46432142674534305, 60.70473504998254555, 1.000000000000003553 ) ) ;
#11013 = EDGE_CURVE ( 'NONE', #29, #7014, #4022, .T. ) ;
#11014 =( REPRESENTATION_RELATIONSHIP ('NONE','NONE', #1997, #5503 ) REPRESENTATION_RELATIONSHIP_WITH_TRANSFORMATION ( #9413 )SHAPE_REPRESENTATION_RELATIONSHIP( ) );
#11015 = DIRECTION ( 'NONE',  ( -0.000000000000000000, 1.000000000000000000, -0.000000000000000000 ) ) ;
#11016 = DIRECTION ( 'NONE',  ( 0.000000000000000000, 0.000000000000000000, 1.000000000000000000 ) ) ;
#11017 = DIRECTION ( 'NONE',  ( 0.000000000000000000, 0.000000000000000000, 1.000000000000000000 ) ) ;
#11018 = ORIENTED_EDGE ( 'NONE', *, *, #5108, .F. ) ;
#11019 = AXIS2_PLACEMENT_3D ( 'NONE', #2384, #5444, #5378 ) ;
#11020 = DIRECTION ( 'NONE',  ( -0.000000000000000000, -0.000000000000000000, -1.000000000000000000 ) ) ;
#11021 = EDGE_LOOP ( 'NONE', ( #10753, #5029, #9336 ) ) ;
#11022 = CARTESIAN_POINT ( 'NONE',  ( 3.800000000000015365, 90.00000000000000000, 4.212500001229034119 ) ) ;
#11023 = CARTESIAN_POINT ( 'NONE',  ( 11.38811426945699701, 73.16316976839823383, 4.000000000000000000 ) ) ;
#11024 = CARTESIAN_POINT ( 'NONE',  ( 45.00000000000000000, 0.000000000000000000, -5.750000000000000000 ) ) ;
#11025 = EDGE_CURVE ( 'NONE', #4194, #11844, #2055, .T. ) ;
#11026 = CARTESIAN_POINT ( 'NONE',  ( 31.50000000000000000, 90.00000000000000000, 4.800000000000000711 ) ) ;
#11027 = AXIS2_PLACEMENT_3D ( 'NONE', #9622, #4905, #11104 ) ;
#11028 = ADVANCED_FACE ( 'NONE', ( #11864 ), #4149, .T. ) ;
#11029 = ORIENTED_EDGE ( 'NONE', *, *, #1831, .F. ) ;
#11030 = CARTESIAN_POINT ( 'NONE',  ( 1.040000000000000036, -0.5773502691896255090, 1.000000000000000000 ) ) ;
#11031 = CARTESIAN_POINT ( 'NONE',  ( 35.00000000000000711, 53.97334320256736362, 3.762500000000000178 ) ) ;
#11032 = ORIENTED_EDGE ( 'NONE', *, *, #7530, .T. ) ;
#11033 = DIRECTION ( 'NONE',  ( -1.000000000000000000, 0.000000000000000000, 0.000000000000000000 ) ) ;
#11034 = ORIENTED_EDGE ( 'NONE', *, *, #8348, .T. ) ;
#11035 = FILL_AREA_STYLE_COLOUR ( '', #1291 ) ;
#11036 = ORIENTED_EDGE ( 'NONE', *, *, #1642, .F. ) ;
#11037 = AXIS2_PLACEMENT_3D ( 'NONE', #12455, #3433, #599 ) ;
#11038 = CARTESIAN_POINT ( 'NONE',  ( 35.00000000000000000, 90.00000000000000000, -3.000000000000000000 ) ) ;
#11039 = CARTESIAN_POINT ( 'NONE',  ( -3.068288344391240763, -2.655262421758692426, -0.8000000000000000444 ) ) ;
#11040 = ORIENTED_EDGE ( 'NONE', *, *, #4122, .T. ) ;
#11041 = EDGE_LOOP ( 'NONE', ( #3088, #5722, #5498, #8381 ) ) ;
#11043 = DIRECTION ( 'NONE',  ( 0.000000000000000000, 0.000000000000000000, -1.000000000000000000 ) ) ;
#11042 = VECTOR ( 'NONE', #12623, 1000.000000000000000 ) ;
#11044 = ORIENTED_EDGE ( 'NONE', *, *, #2567, .T. ) ;
#11045 = CARTESIAN_POINT ( 'NONE',  ( 35.00000000000000000, 126.3079067962035822, 4.690625000614518036 ) ) ;
#11046 = AXIS2_PLACEMENT_3D ( 'NONE', #1113, #5105, #9100 ) ;
#11047 = ORIENTED_EDGE ( 'NONE', *, *, #188, .T. ) ;
#11048 = CARTESIAN_POINT ( 'NONE',  ( 38.50000000000000711, 90.00000000000000000, 4.800000000000000711 ) ) ;
#11049 = EDGE_CURVE ( 'NONE', #12512, #10795, #1859, .T. ) ;
#11050 = ORIENTED_EDGE ( 'NONE', *, *, #10109, .T. ) ;
#11051 = CARTESIAN_POINT ( 'NONE',  ( -36.66666666666665009, 30.00000000000000000, 7.999999999999996447 ) ) ;
#11052 = CARTESIAN_POINT ( 'NONE',  ( 35.00000000000000711, 53.69209320379639649, 3.115625000614517415 ) ) ;
#11053 = DIRECTION ( 'NONE',  ( 0.000000000000000000, -1.000000000000000000, 0.000000000000000000 ) ) ;
#11054 = AXIS2_PLACEMENT_3D ( 'NONE', #12376, #5435, #10545 ) ;
#11055 = CARTESIAN_POINT ( 'NONE',  ( -4.763019983628629994, -4.349268977144818749, -0.8000000000000000444 ) ) ;
#11056 =( NAMED_UNIT ( * ) SI_UNIT ( $, .STERADIAN. ) SOLID_ANGLE_UNIT ( ) );
#11057 = CARTESIAN_POINT ( 'NONE',  ( 35.00000000000000711, 53.97334320256736362, 4.212500000000000355 ) ) ;
#11058 = ORIENTED_EDGE ( 'NONE', *, *, #1544, .F. ) ;
#11059 = CARTESIAN_POINT ( 'NONE',  ( 50.59999999999999432, 117.0199925980744666, 3.050000000000000266 ) ) ;
#11060 = ADVANCED_FACE ( 'NONE', ( #8006 ), #863, .T. ) ;
#11061 = EDGE_CURVE ( 'NONE', #39, #11476, #3897, .T. ) ;
#11062 = DIRECTION ( 'NONE',  ( -0.000000000000000000, -0.000000000000000000, -1.000000000000000000 ) ) ;
#11063 = CARTESIAN_POINT ( 'NONE',  ( 66.20000000000000284, 90.00000000000000000, 6.000000000000000000 ) ) ;
#11064 = ORIENTED_EDGE ( 'NONE', *, *, #8706, .T. ) ;
#11065 = VECTOR ( 'NONE', #6855, 1000.000000000000114 ) ;
#11066 = DIRECTION ( 'NONE',  ( -0.000000000000000000, -1.000000000000000000, -0.000000000000000000 ) ) ;
#11067 = EDGE_CURVE ( 'NONE', #12910, #108, #10938, .T. ) ;
#11068 = EDGE_LOOP ( 'NONE', ( #7788, #12373, #4661, #11378, #11753, #4421 ) ) ;
#11069 = CARTESIAN_POINT ( 'NONE',  ( 35.00000000000000000, 90.00000000000000000, -1.000000000000000000 ) ) ;
#11070 = CARTESIAN_POINT ( 'NONE',  ( 3.556430356250014579, 108.1539533981018053, 3.865625000614517415 ) ) ;
#11071 = ORIENTED_EDGE ( 'NONE', *, *, #7158, .F. ) ;
#11072 = CARTESIAN_POINT ( 'NONE',  ( 50.72178482187499071, 117.2309300971526937, 4.259375000614517681 ) ) ;
#11073 = DIRECTION ( 'NONE',  ( -0.000000000000000000, 1.000000000000000000, -0.000000000000000000 ) ) ;
#11074 = DIRECTION ( 'NONE',  ( -0.9914448613738103822, -0.1305261922200528224, 0.000000000000000000 ) ) ;
#11075 = CONICAL_SURFACE ( 'NONE', #5438, 1.500000000000001332, 1.029744260000000411 ) ;
#11076 =( BOUNDED_SURFACE ( )  B_SPLINE_SURFACE ( 1, 2, ( 
 ( #1649, #5638, #9500, #10480, #11326, #9630, #5504, #8651, #3424, #5371, #4662, #1515, #7602, #1584, #6354, #2508, #12377, #8591, #10353, #10417, #391, #12581, #3689, #9368, #525, #7472, #9566, #12513, #3557, #7538, #2444, #5572, #6417, #3622, #11591, #3492, #591, #12646, #2640, #4598, #6614, #11525, #4403, #8394, #656, #10613, #2571, #6549, #8458, #9431, #4464, #7406, #10549, #11393, #455 ),
 ( #11458, #5949, #9494, #2767, #4974, #12828, #2955, #5828, #6807, #7667, #908, #9757, #7790, #10920, #11847, #9947, #4787, #8961, #12706, #975, #4914, #1905, #8776, #11782, #9689, #722, #3877, #1971, #1843, #11654, #5886, #12769, #9878, #8834, #10801, #2704, #12896, #3810, #6678, #4852, #10674, #6936, #2893, #1714, #7858, #9819, #5702, #4727, #11909, #7730, #6872, #3748, #8712, #10860, #783 ) ),
 .UNSPECIFIED., .F., .F., .F. ) 
 B_SPLINE_SURFACE_WITH_KNOTS ( ( 2, 2 ),
 ( 3, 2, 2, 2, 2, 2, 2, 2, 2, 2, 2, 2, 2, 2, 2, 2, 2, 2, 2, 2, 2, 2, 2, 2, 2, 2, 2, 3 ),
 ( 0.000000000000000000, 1.000000000000000000 ),
 ( 0.000000000000000000, 0.03333333333333333287, 0.06666666666666666574, 0.1000000000000000056, 0.1333333333333333315, 0.1666666666666666574, 0.2000000000000000111, 0.2333333333333333370, 0.2666666666666666630, 0.2999999999999999889, 0.3333333333333333148, 0.3666666666666666408, 0.4000000000000000222, 0.4333333333333333481, 0.4666666666666666741, 0.5000000000000000000, 0.5333333333333333259, 0.5666666666666666519, 0.5999999999999999778, 0.6333333333333333037, 0.6666666666666666297, 0.6999999999999999556, 0.7333333333333332815, 0.7666666666666667185, 0.8000000000000000444, 0.8333333333333333703, 0.8666666666666666963, 0.8887752010635167066 ),
 .UNSPECIFIED. ) 
 GEOMETRIC_REPRESENTATION_ITEM ( )  RATIONAL_B_SPLINE_SURFACE ( (
 ( 1.000000000000000000, 0.8660254037844387076, 1.000000000000000000, 0.8660254037844387076, 1.000000000000000000, 0.8660254037844387076, 1.000000000000000000, 0.8660254037844387076, 1.000000000000000000, 0.8660254037844387076, 1.000000000000000000, 0.8660254037844387076, 1.000000000000000000, 0.8660254037844387076, 1.000000000000000000, 0.8660254037844387076, 1.000000000000000000, 0.8660254037844387076, 1.000000000000000000, 0.8660254037844387076, 1.000000000000000000, 0.8660254037844387076, 1.000000000000000000, 0.8660254037844387076, 1.000000000000000000, 0.8660254037844387076, 1.000000000000000000, 0.8660254037844387076, 1.000000000000000000, 0.8660254037844387076, 1.000000000000000000, 0.8660254037844387076, 1.000000000000000000, 0.8660254037844387076, 1.000000000000000000, 0.8660254037844387076, 1.000000000000000000, 0.8660254037844387076, 1.000000000000000000, 0.8660254037844387076, 1.000000000000000000, 0.8660254037844387076, 1.000000000000000000, 0.8660254037844387076, 1.000000000000000000, 0.8660254037844387076, 1.000000000000000000, 0.8660254037844387076, 1.000000000000000000, 0.8660254037844387076, 1.000000000000000000, 0.8660254037844387076, 1.000000000000000000, 0.9111405409379251807, 0.9401542263054123438),
 ( 1.000000000000000000, 0.8660254037844387076, 1.000000000000000000, 0.8660254037844387076, 1.000000000000000000, 0.8660254037844387076, 1.000000000000000000, 0.8660254037844387076, 1.000000000000000000, 0.8660254037844387076, 1.000000000000000000, 0.8660254037844387076, 1.000000000000000000, 0.8660254037844387076, 1.000000000000000000, 0.8660254037844387076, 1.000000000000000000, 0.8660254037844387076, 1.000000000000000000, 0.8660254037844387076, 1.000000000000000000, 0.8660254037844387076, 1.000000000000000000, 0.8660254037844387076, 1.000000000000000000, 0.8660254037844387076, 1.000000000000000000, 0.8660254037844387076, 1.000000000000000000, 0.8660254037844387076, 1.000000000000000000, 0.8660254037844387076, 1.000000000000000000, 0.8660254037844387076, 1.000000000000000000, 0.8660254037844387076, 1.000000000000000000, 0.8660254037844387076, 1.000000000000000000, 0.8660254037844387076, 1.000000000000000000, 0.8660254037844387076, 1.000000000000000000, 0.8660254037844387076, 1.000000000000000000, 0.8660254037844387076, 1.000000000000000000, 0.8660254037844387076, 1.000000000000000000, 0.8660254037844387076, 1.000000000000000000, 0.8660254037844387076, 1.000000000000000000, 0.9111405409379251807, 0.9401542263054123438) ) ) 
 REPRESENTATION_ITEM ( '' )  SURFACE ( )  );
#11077 = LINE ( 'NONE', #7289, #4279 ) ;
#11078 = EDGE_CURVE ( 'NONE', #2817, #4053, #1, .T. ) ;
#11079 = CYLINDRICAL_SURFACE ( 'NONE', #10945, 4.338286831716297698 ) ;
#11080 = FACE_BOUND ( 'NONE', #10457, .T. ) ;
#11081 = VECTOR ( 'NONE', #11002, 1000.000000000000000 ) ;
#11082 = LINE ( 'NONE', #3185, #6270 ) ;
#11083 = DIRECTION ( 'NONE',  ( 0.000000000000000000, 0.8660254037844387076, -0.4999999999999998890 ) ) ;
#11084 = ORIENTED_EDGE ( 'NONE', *, *, #11956, .F. ) ;
#11085 = LINE ( 'NONE', #5068, #6830 ) ;
#11086 = ORIENTED_EDGE ( 'NONE', *, *, #7435, .F. ) ;
#11087 = VECTOR ( 'NONE', #8903, 1000.000000000000000 ) ;
#11088 = CARTESIAN_POINT ( 'NONE',  ( 4.336808689942017736E-16, -1.424999999999999822, -2.617682533177465074E-16 ) ) ;
#11089 = CARTESIAN_POINT ( 'NONE',  ( 3.800000000000015365, 90.00000000000000000, 4.212500001229034119 ) ) ;
#11090 = EDGE_CURVE ( 'NONE', #5692, #10905, #2257, .T. ) ;
#11091 = CARTESIAN_POINT ( 'NONE',  ( 0.000000000000000000, 30.00000000000000000, 0.000000000000000000 ) ) ;
#11092 = ORIENTED_EDGE ( 'NONE', *, *, #10761, .F. ) ;
#11093 = CARTESIAN_POINT ( 'NONE',  ( 45.00000000000000000, 0.000000000000000000, 5.750000000000000888 ) ) ;
#11094 = LINE ( 'NONE', #12218, #4812 ) ;
#11095 = EDGE_LOOP ( 'NONE', ( #2015, #7195, #484, #1711 ) ) ;
#11096 = SURFACE_STYLE_FILL_AREA ( #2220 ) ;
#11097 = SURFACE_STYLE_USAGE ( .BOTH. , #3137 ) ;
#11098 = ORIENTED_EDGE ( 'NONE', *, *, #10741, .T. ) ;
#11099 = CARTESIAN_POINT ( 'NONE',  ( 0.000000000000000000, 0.000000000000000000, 0.000000000000000000 ) ) ;
#11100 = ORIENTED_EDGE ( 'NONE', *, *, #1677, .T. ) ;
#11101 = EDGE_CURVE ( 'NONE', #4578, #3991, #2321, .T. ) ;
#11102 = EDGE_CURVE ( 'NONE', #5885, #9895, #6698, .T. ) ;
#11103 = FACE_OUTER_BOUND ( 'NONE', #11808, .T. ) ;
#11104 = DIRECTION ( 'NONE',  ( -1.000000000000000000, 0.000000000000000000, -5.337610695313252124E-17 ) ) ;
#11105 = ORIENTED_EDGE ( 'NONE', *, *, #10184, .T. ) ;
#11106 = VERTEX_POINT ( 'NONE', #9370 ) ;
#11107 = AXIS2_PLACEMENT_3D ( 'NONE', #3483, #11315, #9360 ) ;
#11108 = CARTESIAN_POINT ( 'NONE',  ( -23.49999999999999289, 53.38268590218009280, 3.000000000000000000 ) ) ;
#11109 = ORIENTED_EDGE ( 'NONE', *, *, #7973, .F. ) ;
#11110 = DIRECTION ( 'NONE',  ( 0.000000000000000000, 0.000000000000000000, 1.000000000000000000 ) ) ;
#11111 = CARTESIAN_POINT ( 'NONE',  ( 19.40000000000000924, 117.0199925980744666, 4.587500001229034119 ) ) ;
#11112 = ORIENTED_EDGE ( 'NONE', *, *, #8542, .T. ) ;
#11113 = CARTESIAN_POINT ( 'NONE',  ( 48.49999999999995737, 86.00000000000000000, -8.000000000000000000 ) ) ;
#11114 = CARTESIAN_POINT ( 'NONE',  ( -9.666666666666657193, 59.05996354921150271, 3.000000000000058176 ) ) ;
#11115 = VERTEX_POINT ( 'NONE', #1192 ) ;
#11116 = LINE ( 'NONE', #12368, #8605 ) ;
#11117 = CARTESIAN_POINT ( 'NONE',  ( 3.556430356250015024, 90.00000000000000000, 3.453125000614517770 ) ) ;
#11118 = AXIS2_PLACEMENT_3D ( 'NONE', #9209, #1355, #2228 ) ;
#11119 = CARTESIAN_POINT ( 'NONE',  ( 35.75000000000000711, 93.41869858279433458, -8.000000000000000000 ) ) ;
#11120 = DIRECTION ( 'NONE',  ( -0.000000000000000000, -0.000000000000000000, -1.000000000000000000 ) ) ;
#11121 = EDGE_CURVE ( 'NONE', #11833, #1436, #11329, .T. ) ;
#11122 = ORIENTED_EDGE ( 'NONE', *, *, #2370, .F. ) ;
#11123 = CARTESIAN_POINT ( 'NONE',  ( 35.00000000000000000, 126.0266567974326222, 3.087499999999999911 ) ) ;
#11124 = EDGE_LOOP ( 'NONE', ( #10027, #68, #10055, #5622 ) ) ;
#11125 = DIRECTION ( 'NONE',  ( 0.000000000000000000, 0.000000000000000000, 1.000000000000000000 ) ) ;
#11126 = LINE ( 'NONE', #6158, #11795 ) ;
#11127 = VERTEX_POINT ( 'NONE', #11205 ) ;
#11128 = DIRECTION ( 'NONE',  ( 0.000000000000000000, -0.000000000000000000, 1.000000000000000000 ) ) ;
#11129 = EDGE_LOOP ( 'NONE', ( #12823, #6418, #12801, #11295, #12498, #6889 ) ) ;
#11130 = FACE_OUTER_BOUND ( 'NONE', #3873, .T. ) ;
#11131 = CIRCLE ( 'NONE', #3427, 0.9999999999999991118 ) ;
#11132 = UNCERTAINTY_MEASURE_WITH_UNIT (LENGTH_MEASURE( 1.000000000000000082E-05 ), #10316, 'distance_accuracy_value', 'NONE');
#11133 = CARTESIAN_POINT ( 'NONE',  ( 3.556430356250014579, 108.1539533981018053, 3.415625000614517237 ) ) ;
#11134 = ORIENTED_EDGE ( 'NONE', *, *, #11744, .F. ) ;
#11135 = CARTESIAN_POINT ( 'NONE',  ( 50.72178482187501203, 62.76906990284730625, 4.559375000614517504 ) ) ;
#11136 = CARTESIAN_POINT ( 'NONE',  ( 5.011331584521383498, 81.39071625125095011, 5.000000000000000000 ) ) ;
#11137 = DIRECTION ( 'NONE',  ( 0.000000000000000000, 0.000000000000000000, 1.000000000000000000 ) ) ;
#11138 =( GEOMETRIC_REPRESENTATION_CONTEXT ( 3 ) GLOBAL_UNCERTAINTY_ASSIGNED_CONTEXT ( ( #3037 ) ) GLOBAL_UNIT_ASSIGNED_CONTEXT ( ( #7177, #5932, #228 ) ) REPRESENTATION_CONTEXT ( 'NONE', 'WORKASPACE' ) );
#11139 = ADVANCED_FACE ( 'NONE', ( #3495 ), #2379, .T. ) ;
#11140 = LINE ( 'NONE', #6367, #10749 ) ;
#11141 = VECTOR ( 'NONE', #3710, 999.9999999999998863 ) ;
#11142 = LINE ( 'NONE', #12134, #9172 ) ;
#11143 = CARTESIAN_POINT ( 'NONE',  ( 48.49999999999995737, 90.00000000000000000, -5.000000000000000000 ) ) ;
#11144 = DIRECTION ( 'NONE',  ( -0.000000000000000000, -0.5000000000000003331, -0.8660254037844383745 ) ) ;
#11145 = AXIS2_PLACEMENT_3D ( 'NONE', #7333, #2371, #6346 ) ;
#11146 = CARTESIAN_POINT ( 'NONE',  ( 1.040000000000000036, 0.000000000000000000, 2.000000000000000000 ) ) ;
#11147 = PLANE ( 'NONE',  #123 ) ;
#11148 = ORIENTED_EDGE ( 'NONE', *, *, #11340, .F. ) ;
#11149 = DIRECTION ( 'NONE',  ( -1.000000000000000000, 0.000000000000000000, 0.000000000000000000 ) ) ;
#11150 = EDGE_LOOP ( 'NONE', ( #7852, #2372, #2755, #3267 ) ) ;
#11151 = VECTOR ( 'NONE', #5518, 1000.000000000000000 ) ;
#11152 = EDGE_CURVE ( 'NONE', #10011, #7510, #2447, .T. ) ;
#11153 = SURFACE_STYLE_USAGE ( .BOTH. , #5071 ) ;
#11154 = VECTOR ( 'NONE', #4750, 1000.000000000000114 ) ;
#11155 = ADVANCED_FACE ( 'NONE', ( #7409 ), #7282, .T. ) ;
#11156 = DIRECTION ( 'NONE',  ( 0.000000000000000000, 0.000000000000000000, 1.000000000000000000 ) ) ;
#11157 = FACE_OUTER_BOUND ( 'NONE', #199, .T. ) ;
#11158 = CARTESIAN_POINT ( 'NONE',  ( 65.00000000000000000, 90.00000000000000000, 1.000000000000003553 ) ) ;
#11159 = UNCERTAINTY_MEASURE_WITH_UNIT (LENGTH_MEASURE( 1.000000000000000082E-05 ), #11955, 'distance_accuracy_value', 'NONE');
#11160 = ORIENTED_EDGE ( 'NONE', *, *, #9257, .F. ) ;
#11161 = VECTOR ( 'NONE', #2426, 1000.000000000000000 ) ;
#11162 = DIRECTION ( 'NONE',  ( -1.000000000000000000, 0.000000000000000000, 0.000000000000000000 ) ) ;
#11163 = DIRECTION ( 'NONE',  ( 1.000000000000000000, 0.000000000000000000, -0.000000000000000000 ) ) ;
#11164 = CIRCLE ( 'NONE', #8047, 28.99999999999999289 ) ;
#11165 = ORIENTED_EDGE ( 'NONE', *, *, #12642, .T. ) ;
#11166 = DIRECTION ( 'NONE',  ( 0.000000000000000000, 0.000000000000000000, -1.000000000000000000 ) ) ;
#11167 = VERTEX_POINT ( 'NONE', #1319 ) ;
#11168 = CARTESIAN_POINT ( 'NONE',  ( 17.55098605904792564, 66.83414348997642662, 1.000000000000003109 ) ) ;
#11169 = ORIENTED_EDGE ( 'NONE', *, *, #8611, .T. ) ;
#11170 = EDGE_CURVE ( 'NONE', #9866, #8130, #331, .T. ) ;
#11171 = FACE_OUTER_BOUND ( 'NONE', #10901, .T. ) ;
#11172 = CARTESIAN_POINT ( 'NONE',  ( 32.09707732552327286, 88.32801317409231956, -3.800000000000000266 ) ) ;
#11173 = AXIS2_PLACEMENT_3D ( 'NONE', #11093, #4306, #11227 ) ;
#11174 = ORIENTED_EDGE ( 'NONE', *, *, #8951, .F. ) ;
#11175 = AXIS2_PLACEMENT_3D ( 'NONE', #828, #6721, #2681 ) ;
#11176 = EDGE_LOOP ( 'NONE', ( #8042, #1469, #12231, #9599, #11856, #1231 ) ) ;
#11177 = CYLINDRICAL_SURFACE ( 'NONE', #1362, 30.19999999999998863 ) ;
#11178 = ORIENTED_EDGE ( 'NONE', *, *, #6595, .T. ) ;
#11179 = DIRECTION ( 'NONE',  ( 1.214306433183764966E-17, -1.000000000000000000, 0.000000000000000000 ) ) ;
#11180 = CARTESIAN_POINT ( 'NONE',  ( 35.00000000000000711, 53.97334320256736362, 4.325000001229033941 ) ) ;
#11181 = EDGE_CURVE ( 'NONE', #6728, #5916, #8384, .T. ) ;
#11182 = VERTEX_POINT ( 'NONE', #10419 ) ;
#11183 = VECTOR ( 'NONE', #11407, 1000.000000000000000 ) ;
#11184 = PLANE ( 'NONE',  #7797 ) ;
#11185 = PRODUCT_DEFINITION_SHAPE ( 'NONE', 'NONE',  #12964 ) ;
#11186 = CARTESIAN_POINT ( 'NONE',  ( 0.000000000000000000, 0.000000000000000000, 10.00000000000000000 ) ) ;
#11187 = ORIENTED_EDGE ( 'NONE', *, *, #7674, .F. ) ;
#11188 = CIRCLE ( 'NONE', #4510, 10.00000000000000178 ) ;
#11189 = FACE_OUTER_BOUND ( 'NONE', #12360, .T. ) ;
#11190 = CARTESIAN_POINT ( 'NONE',  ( 66.44356964374998142, 108.1539533981018053, 4.165625000614516793 ) ) ;
#11191 = DIRECTION ( 'NONE',  ( 1.000000000000000000, 0.000000000000000000, 0.000000000000000000 ) ) ;
#11192 = CARTESIAN_POINT ( 'NONE',  ( 35.00000000000000711, 53.97334320256736362, 2.975000001229034741 ) ) ;
#11193 =( NAMED_UNIT ( * ) SI_UNIT ( $, .STERADIAN. ) SOLID_ANGLE_UNIT ( ) );
#11194 = CIRCLE ( 'NONE', #7230, 0.5999999999999999778 ) ;
#11195 = FACE_OUTER_BOUND ( 'NONE', #1746, .T. ) ;
#11196 = ORIENTED_EDGE ( 'NONE', *, *, #6536, .F. ) ;
#11197 = VECTOR ( 'NONE', #12611, 1000.000000000000000 ) ;
#11198 = CARTESIAN_POINT ( 'NONE',  ( 3.800000000000015365, 108.0133283987163111, 3.612500000000000711 ) ) ;
#11199 = ORIENTED_EDGE ( 'NONE', *, *, #6714, .F. ) ;
#11200 = CARTESIAN_POINT ( 'NONE',  ( 35.75000000000000711, 93.26496554346289258, -3.799999999999999822 ) ) ;
#11201 = ORIENTED_EDGE ( 'NONE', *, *, #4981, .T. ) ;
#11202 = EDGE_CURVE ( 'NONE', #6201, #7668, #634, .T. ) ;
#11203 = DIRECTION ( 'NONE',  ( 0.000000000000000000, 0.000000000000000000, 1.000000000000000000 ) ) ;
#11204 = ORIENTED_EDGE ( 'NONE', *, *, #1425, .T. ) ;
#11205 = CARTESIAN_POINT ( 'NONE',  ( 31.65768047819777919, 88.96129878493390208, 4.000000000000000000 ) ) ;
#11206 = CARTESIAN_POINT ( 'NONE',  ( 66.44356964374999563, 90.00000000000000000, 3.228125000614517237 ) ) ;
#11207 = AXIS2_PLACEMENT_3D ( 'NONE', #610, #7554, #8347 ) ;
#11208 = CARTESIAN_POINT ( 'NONE',  ( 3.556430356250028790, 71.84604660189818048, 3.996875000614517504 ) ) ;
#11209 = DIRECTION ( 'NONE',  ( 0.000000000000000000, 0.000000000000000000, -1.000000000000000000 ) ) ;
#11210 = DIRECTION ( 'NONE',  ( 0.000000000000000000, -1.000000000000000000, 0.000000000000000000 ) ) ;
#11211 = DIRECTION ( 'NONE',  ( 0.000000000000000000, 0.000000000000000000, 1.000000000000000000 ) ) ;
#11212 = CARTESIAN_POINT ( 'NONE',  ( 35.75000000000000711, 93.26496554346289258, -3.799999999999999822 ) ) ;
#11213 = CARTESIAN_POINT ( 'NONE',  ( 41.46432142674534305, 60.70473504998254555, -3.000000000000000000 ) ) ;
#11214 = VECTOR ( 'NONE', #11914, 1000.000000000000000 ) ;
#11215 = CARTESIAN_POINT ( 'NONE',  ( -16.33333333333332504, 46.12451549659709116, -7.999999999999996447 ) ) ;
#11216 = LINE ( 'NONE', #344, #9407 ) ;
#11217 = CARTESIAN_POINT ( 'NONE',  ( 0.000000000000000000, 0.4117131682837005258, -0.8000000000000000444 ) ) ;
#11218 = ADVANCED_FACE ( 'NONE', ( #11130 ), #9433, .T. ) ;
#11219 = ORIENTED_EDGE ( 'NONE', *, *, #6043, .F. ) ;
#11220 = CARTESIAN_POINT ( 'NONE',  ( -60.00000000000000000, 30.00000000000000000, -2.500000000000000000 ) ) ;
#11221 = VERTEX_POINT ( 'NONE', #1260 ) ;
#11222 = VECTOR ( 'NONE', #9388, 1000.000000000000000 ) ;
#11223 = FACE_OUTER_BOUND ( 'NONE', #1297, .T. ) ;
#11224 = CARTESIAN_POINT ( 'NONE',  ( 35.49999999999995026, 119.9958330439412890, -0.9999999999999970024 ) ) ;
#11225 = CARTESIAN_POINT ( 'NONE',  ( 1.040000000000000036, 0.5773502691896262862, -1.000000000000000000 ) ) ;
#11226 = ORIENTED_EDGE ( 'NONE', *, *, #5564, .T. ) ;
#11227 = DIRECTION ( 'NONE',  ( 0.000000000000000000, 0.000000000000000000, 1.000000000000000000 ) ) ;
#11228 = LINE ( 'NONE', #2146, #6477 ) ;
#11229 = EDGE_CURVE ( 'NONE', #8114, #6389, #1690, .T. ) ;
#11230 = CONICAL_SURFACE ( 'NONE', #3934, 1.500000000000001332, 1.029744260000000411 ) ;
#11231 = ORIENTED_EDGE ( 'NONE', *, *, #3443, .F. ) ;
#11232 = DIRECTION ( 'NONE',  ( 0.000000000000000000, 0.000000000000000000, 1.000000000000000000 ) ) ;
#11233 = CYLINDRICAL_SURFACE ( 'NONE', #5559, 31.19999999999999929 ) ;
#11234 = EDGE_CURVE ( 'NONE', #1698, #9740, #5316, .T. ) ;
#11235 = ORIENTED_EDGE ( 'NONE', *, *, #11434, .F. ) ;
#11236 = VERTEX_POINT ( 'NONE', #4214 ) ;
#11237 = PLANE ( 'NONE',  #11118 ) ;
#11238 = DIRECTION ( 'NONE',  ( 0.000000000000000000, 0.000000000000000000, -1.000000000000000000 ) ) ;
#11239 = AXIS2_PLACEMENT_3D ( 'NONE', #89, #10047, #1880 ) ;
#11240 = ORIENTED_EDGE ( 'NONE', *, *, #12321, .T. ) ;
#11241 = VECTOR ( 'NONE', #1641, 1000.000000000000000 ) ;
#11242 = ORIENTED_EDGE ( 'NONE', *, *, #4742, .F. ) ;
#11243 = DIRECTION ( 'NONE',  ( -1.000000000000000000, 0.000000000000000000, 0.000000000000000000 ) ) ;
#11244 = ORIENTED_EDGE ( 'NONE', *, *, #3494, .T. ) ;
#11245 = APPLICATION_PROTOCOL_DEFINITION ( 'draft international standard', 'automotive_design', 1998, #12541 ) ;
#11246 = CARTESIAN_POINT ( 'NONE',  ( 19.27821517812503060, 62.76906990284727783, 3.528125000614517059 ) ) ;
#11247 = ADVANCED_FACE ( 'NONE', ( #262 ), #12138, .T. ) ;
#11248 = VERTEX_POINT ( 'NONE', #9308 ) ;
#11249 = LINE ( 'NONE', #5359, #6037 ) ;
#11250 = VERTEX_POINT ( 'NONE', #12257 ) ;
#11251 = AXIS2_PLACEMENT_3D ( 'NONE', #11840, #8643, #2886 ) ;
#11252 = DIRECTION ( 'NONE',  ( 0.000000000000000000, 0.000000000000000000, 1.000000000000000000 ) ) ;
#11253 = DIRECTION ( 'NONE',  ( 0.000000000000000000, -1.000000000000000000, -0.000000000000000000 ) ) ;
#11254 = CARTESIAN_POINT ( 'NONE',  ( 50.59999999999999432, 117.0199925980744666, 3.162500001229034741 ) ) ;
#11255 = LINE ( 'NONE', #3025, #11896 ) ;
#11256 = VECTOR ( 'NONE', #10402, 1000.000000000000000 ) ;
#11257 = VERTEX_POINT ( 'NONE', #3305 ) ;
#11258 = CARTESIAN_POINT ( 'NONE',  ( 66.19999999999997442, 108.0133283987163253, 4.362499999999999822 ) ) ;
#11259 = ORIENTED_EDGE ( 'NONE', *, *, #1077, .T. ) ;
#11260 = DIRECTION ( 'NONE',  ( -0.000000000000000000, -0.000000000000000000, -1.000000000000000000 ) ) ;
#11261 = ADVANCED_FACE ( 'NONE', ( #8333 ), #8990, .F. ) ;
#11262 = VERTEX_POINT ( 'NONE', #7345 ) ;
#11263 = CARTESIAN_POINT ( 'NONE',  ( -4.270088556250601699E-16, 2.000000000000000000, 8.000000000000000000 ) ) ;
#11264 = PRODUCT_DEFINITION_SHAPE ( 'NONE', 'NONE',  #9854 ) ;
#11265 = ORIENTED_EDGE ( 'NONE', *, *, #5057, .F. ) ;
#11266 = AXIS2_PLACEMENT_3D ( 'NONE', #7277, #4079, #9234 ) ;
#11267 = DIRECTION ( 'NONE',  ( 0.000000000000000000, 0.000000000000000000, 1.000000000000000000 ) ) ;
#11268 = DIRECTION ( 'NONE',  ( 0.000000000000000000, 0.000000000000000000, 1.000000000000000000 ) ) ;
#11269 = AXIS2_PLACEMENT_3D ( 'NONE', #9033, #7271, #983 ) ;
#11270 = CARTESIAN_POINT ( 'NONE',  ( 40.00000000000000000, 0.000000000000000000, 10.00000000000000000 ) ) ;
#11271 = LINE ( 'NONE', #2325, #6428 ) ;
#11272 = EDGE_CURVE ( 'NONE', #12892, #9866, #10882, .T. ) ;
#11273 = CARTESIAN_POINT ( 'NONE',  ( 64.85903780527353035, 87.09520029206045422, -0.9999999999999970024 ) ) ;
#11274 = EDGE_CURVE ( 'NONE', #9327, #1939, #7121, .T. ) ;
#11275 =( BOUNDED_CURVE ( )  B_SPLINE_CURVE ( 2, ( #9727, #10588, #12681, #3720, #6457, #8430, #7703 ),
 .UNSPECIFIED., .F., .F. ) 
 B_SPLINE_CURVE_WITH_KNOTS ( ( 3, 2, 2, 3 ),
 ( 0.3000000000000002109, 0.3333333333333334259, 0.3666666666666666963, 0.3999999999999999667 ),
 .UNSPECIFIED. ) 
 CURVE ( )  GEOMETRIC_REPRESENTATION_ITEM ( )  RATIONAL_B_SPLINE_CURVE ( ( 0.9999999999999991118, 0.8660254037844395958, 1.000000000000000000, 0.8660254037844387076, 1.000000000000000000, 0.8660254037844389297, 0.9999999999999997780 ) ) 
 REPRESENTATION_ITEM ( '' )  );
#11276 = VECTOR ( 'NONE', #1757, 1000.000000000000000 ) ;
#11277 = SURFACE_STYLE_USAGE ( .BOTH. , #7227 ) ;
#11278 = FACE_OUTER_BOUND ( 'NONE', #2631, .T. ) ;
#11279 = CARTESIAN_POINT ( 'NONE',  ( 30.00000000000000711, 0.000000000000000000, 10.00000000000000000 ) ) ;
#11280 = CARTESIAN_POINT ( 'NONE',  ( 2.179634403564814971, -5.614030811971695734, -0.8000000000000000444 ) ) ;
#11281 = LINE ( 'NONE', #11342, #8985 ) ;
#11282 = DIRECTION ( 'NONE',  ( 0.000000000000000000, -1.000000000000000000, 0.000000000000000000 ) ) ;
#11283 = ORIENTED_EDGE ( 'NONE', *, *, #9316, .T. ) ;
#11284 = VECTOR ( 'NONE', #3053, 1000.000000000000000 ) ;
#11285 = CARTESIAN_POINT ( 'NONE',  ( -48.33333333333332860, 0.000000000000000000, -1.734723475976807094E-15 ) ) ;
#11286 = VERTEX_POINT ( 'NONE', #2770 ) ;
#11287 = CARTESIAN_POINT ( 'NONE',  ( -6.666666666666660745, -5.000000000000000000, 0.000000000000000000 ) ) ;
#11288 = DIRECTION ( 'NONE',  ( 0.9510565162951530871, 0.3090169943749492276, 0.000000000000000000 ) ) ;
#11289 = EDGE_CURVE ( 'NONE', #255, #12446, #12568, .T. ) ;
#11290 = LINE ( 'NONE', #8223, #8850 ) ;
#11291 = AXIS2_PLACEMENT_3D ( 'NONE', #11069, #5052, #4993 ) ;
#11292 = VERTEX_POINT ( 'NONE', #11595 ) ;
#11293 = DIRECTION ( 'NONE',  ( 1.000000000000000000, 0.000000000000000000, -0.000000000000000000 ) ) ;
#11294 = CARTESIAN_POINT ( 'NONE',  ( 0.1038759689922479496, -3.348389132562988646, -0.8000000000000000444 ) ) ;
#11295 = ORIENTED_EDGE ( 'NONE', *, *, #3724, .T. ) ;
#11296 = CARTESIAN_POINT ( 'NONE',  ( 65.00000000000000000, 90.00000000000000000, -3.000000000000000000 ) ) ;
#11297 = ORIENTED_EDGE ( 'NONE', *, *, #4120, .T. ) ;
#11298 = ORIENTED_EDGE ( 'NONE', *, *, #7437, .F. ) ;
#11299 = DIRECTION ( 'NONE',  ( 1.000000000000000000, 0.000000000000000000, 0.000000000000000000 ) ) ;
#11300 = VECTOR ( 'NONE', #6474, 1000.000000000000000 ) ;
#11301 = CARTESIAN_POINT ( 'NONE',  ( -6.666666666666660745, -5.000000000000000000, 0.000000000000000000 ) ) ;
#11302 = ADVANCED_FACE ( 'NONE', ( #9568 ), #9633, .F. ) ;
#11303 = ORIENTED_EDGE ( 'NONE', *, *, #6631, .F. ) ;
#11304 = EDGE_CURVE ( 'NONE', #3688, #11641, #6681, .T. ) ;
#11305 = ORIENTED_EDGE ( 'NONE', *, *, #3674, .T. ) ;
#11306 = DIRECTION ( 'NONE',  ( -0.000000000000000000, 1.000000000000000000, -0.000000000000000000 ) ) ;
#11307 = ORIENTED_EDGE ( 'NONE', *, *, #462, .F. ) ;
#11308 = DIRECTION ( 'NONE',  ( 0.000000000000000000, 0.000000000000000000, 1.000000000000000000 ) ) ;
#11309 = CARTESIAN_POINT ( 'NONE',  ( 66.20000000000000284, 71.98667160128370313, 3.500000001229034208 ) ) ;
#11310 = ORIENTED_EDGE ( 'NONE', *, *, #663, .T. ) ;
#11311 = AXIS2_PLACEMENT_3D ( 'NONE', #12397, #5523, #11413 ) ;
#11312 = FACE_OUTER_BOUND ( 'NONE', #2937, .T. ) ;
#11313 = EDGE_LOOP ( 'NONE', ( #8423, #4087, #12507, #10437 ) ) ;
#11314 = CARTESIAN_POINT ( 'NONE',  ( 30.00000000000000711, 2.000000000000000000, -10.00000000000000000 ) ) ;
#11315 = DIRECTION ( 'NONE',  ( 0.000000000000000000, 0.000000000000000000, 1.000000000000000000 ) ) ;
#11316 = CARTESIAN_POINT ( 'NONE',  ( -4.338286831716297698, 0.4117131682837010809, 0.000000000000000000 ) ) ;
#11317 = SURFACE_SIDE_STYLE ('',( #3226 ) ) ;
#11318 = EDGE_CURVE ( 'NONE', #108, #4396, #2841, .T. ) ;
#11319 = AXIS2_PLACEMENT_3D ( 'NONE', #4667, #10554, #1588 ) ;
#11320 = CARTESIAN_POINT ( 'NONE',  ( -53.33333333333332149, 36.15840287135605990, 3.000000000000000000 ) ) ;
#11321 = ORIENTED_EDGE ( 'NONE', *, *, #5202, .T. ) ;
#11322 = CARTESIAN_POINT ( 'NONE',  ( 66.44356964374999563, 90.00000000000000000, 3.734375000614516882 ) ) ;
#11323 = ORIENTED_EDGE ( 'NONE', *, *, #12302, .F. ) ;
#11324 = CARTESIAN_POINT ( 'NONE',  ( 64.24207199149496716, 100.8784753363798075, 2.999999999999999556 ) ) ;
#11325 = ORIENTED_EDGE ( 'NONE', *, *, #6088, .T. ) ;
#11326 = CARTESIAN_POINT ( 'NONE',  ( 50.72178482187499071, 117.2309300971526937, 4.709375000614516971 ) ) ;
#11327 = ORIENTED_EDGE ( 'NONE', *, *, #4154, .T. ) ;
#11328 = AXIS2_PLACEMENT_3D ( 'NONE', #8304, #12354, #7120 ) ;
#11329 = LINE ( 'NONE', #12449, #3163 ) ;
#11330 = LINE ( 'NONE', #2448, #9540 ) ;
#11331 = CARTESIAN_POINT ( 'NONE',  ( 66.44356964374998142, 108.1539533981018053, 3.771875000614516082 ) ) ;
#11332 = CARTESIAN_POINT ( 'NONE',  ( 66.44356964374999563, 90.00000000000000000, 4.578125000614516438 ) ) ;
#11333 = EDGE_CURVE ( 'NONE', #3209, #5137, #11527, .T. ) ;
#11334 = CARTESIAN_POINT ( 'NONE',  ( 35.00000000000000000, 90.00000000000000000, 6.000000000000000000 ) ) ;
#11335 = LINE ( 'NONE', #2578, #12734 ) ;
#11336 = AXIS2_PLACEMENT_3D ( 'NONE', #12697, #3546, #8641 ) ;
#11337 = DIRECTION ( 'NONE',  ( -0.000000000000000000, -0.000000000000000000, -1.000000000000000000 ) ) ;
#11338 = CARTESIAN_POINT ( 'NONE',  ( 5.000000000000004441, 30.00000000000000000, -10.00000000000000000 ) ) ;
#11339 = CARTESIAN_POINT ( 'NONE',  ( -6.666666666666660745, 2.000000000000001332, 0.000000000000000000 ) ) ;
#11340 = EDGE_CURVE ( 'NONE', #10832, #2101, #5506, .T. ) ;
#11341 = EDGE_CURVE ( 'NONE', #4076, #10466, #10677, .T. ) ;
#11342 = CARTESIAN_POINT ( 'NONE',  ( 0.1038759689922479496, -3.348389132562988646, -0.8000000000000000444 ) ) ;
#11343 = DIRECTION ( 'NONE',  ( -5.624500927088228034E-17, 1.370729058197317775E-18, 1.000000000000000000 ) ) ;
#11344 = ORIENTED_EDGE ( 'NONE', *, *, #1861, .T. ) ;
#11345 =( BOUNDED_CURVE ( )  B_SPLINE_CURVE ( 2, ( #2270, #9448, #12392, #473, #10369, #2524, #3509 ),
 .UNSPECIFIED., .F., .F. ) 
 B_SPLINE_CURVE_WITH_KNOTS ( ( 3, 2, 2, 3 ),
 ( 0.000000000000000000, 0.03333333333333339532, 0.06666666666666679064, 0.1000000000000001860 ),
 .UNSPECIFIED. ) 
 CURVE ( )  GEOMETRIC_REPRESENTATION_ITEM ( )  RATIONAL_B_SPLINE_CURVE ( ( 1.000000000000000000, 0.8660254037844387076, 1.000000000000000000, 0.8660254037844387076, 1.000000000000000000, 0.8660254037844380415, 1.000000000000000666 ) ) 
 REPRESENTATION_ITEM ( '' )  );
#11346 = FACE_OUTER_BOUND ( 'NONE', #4973, .T. ) ;
#11347 = ORIENTED_EDGE ( 'NONE', *, *, #4582, .F. ) ;
#11348 = PRESENTATION_STYLE_ASSIGNMENT (( #12340 ) ) ;
#11349 = AXIS2_PLACEMENT_3D ( 'NONE', #353, #12213, #11288 ) ;
#11350 = ADVANCED_FACE ( 'NONE', ( #4534 ), #10482, .T. ) ;
#11351 = LINE ( 'NONE', #5395, #3440 ) ;
#11352 = LINE ( 'NONE', #4556, #5960 ) ;
#11353 = FACE_OUTER_BOUND ( 'NONE', #861, .T. ) ;
#11354 =( GEOMETRIC_REPRESENTATION_CONTEXT ( 3 ) GLOBAL_UNCERTAINTY_ASSIGNED_CONTEXT ( ( #4655 ) ) GLOBAL_UNIT_ASSIGNED_CONTEXT ( ( #3024, #10759, #3160 ) ) REPRESENTATION_CONTEXT ( 'NONE', 'WORKASPACE' ) );
#11355 = ORIENTED_EDGE ( 'NONE', *, *, #4413, .F. ) ;
#11356 = ADVANCED_BREP_SHAPE_REPRESENTATION ( '', ( #12113, #5704 ), #3631 ) ;
#11357 = FACE_OUTER_BOUND ( 'NONE', #4642, .T. ) ;
#11358 = CARTESIAN_POINT ( 'NONE',  ( 21.49999999999998579, 90.00000000000000000, -10.00000000000000000 ) ) ;
#11359 = EDGE_CURVE ( 'NONE', #6548, #4634, #5705, .T. ) ;
#11360 = EDGE_LOOP ( 'NONE', ( #11105, #3924, #8816, #8250, #10514, #4823 ) ) ;
#11361 = VECTOR ( 'NONE', #10049, 1000.000000000000000 ) ;
#11362 = DIRECTION ( 'NONE',  ( 1.000000000000000000, 0.000000000000000000, 0.000000000000000000 ) ) ;
#11363 = ORIENTED_EDGE ( 'NONE', *, *, #1766, .T. ) ;
#11364 = ORIENTED_EDGE ( 'NONE', *, *, #739, .T. ) ;
#11365 = LINE ( 'NONE', #8106, #3200 ) ;
#11366 = CARTESIAN_POINT ( 'NONE',  ( 1.040000000000000036, 0.5773502691896263972, 1.000000000000000000 ) ) ;
#11367 = ORIENTED_EDGE ( 'NONE', *, *, #10619, .T. ) ;
#11368 = VECTOR ( 'NONE', #12068, 1000.000000000000000 ) ;
#11369 = ORIENTED_EDGE ( 'NONE', *, *, #7198, .T. ) ;
#11370 = CARTESIAN_POINT ( 'NONE',  ( 4.800000000000015810, 90.00000000000000000, -5.000000000000000000 ) ) ;
#11371 = ORIENTED_EDGE ( 'NONE', *, *, #364, .T. ) ;
#11372 = LINE ( 'NONE', #7454, #11161 ) ;
#11373 = ITEM_DEFINED_TRANSFORMATION ( 'NONE', 'NONE', #5086,  #5704 ) ;
#11374 = CARTESIAN_POINT ( 'NONE',  ( 19.40000000000002700, 62.98000740192551206, 4.287500001229034297 ) ) ;
#11375 = ORIENTED_EDGE ( 'NONE', *, *, #6921, .T. ) ;
#11376 = EDGE_CURVE ( 'NONE', #11634, #237, #2546, .T. ) ;
#11377 = LINE ( 'NONE', #6278, #5198 ) ;
#11378 = ORIENTED_EDGE ( 'NONE', *, *, #9329, .T. ) ;
#11379 = CYLINDRICAL_SURFACE ( 'NONE', #4220, 1.499999999999999556 ) ;
#11381 = ORIENTED_EDGE ( 'NONE', *, *, #12451, .F. ) ;
#11380 = VECTOR ( 'NONE', #9990, 1000.000000000000000 ) ;
#11382 = EDGE_CURVE ( 'NONE', #7638, #8608, #6551, .T. ) ;
#11383 = VECTOR ( 'NONE', #971, 1000.000000000000000 ) ;
#11384 = CARTESIAN_POINT ( 'NONE',  ( 66.19999999999988916, 71.98667160128361786, 4.737499999999998934 ) ) ;
#11385 = DIRECTION ( 'NONE',  ( 1.445602896647339656E-17, -0.000000000000000000, 1.000000000000000000 ) ) ;
#11386 = PRESENTATION_STYLE_ASSIGNMENT (( #1442 ) ) ;
#11387 = ORIENTED_EDGE ( 'NONE', *, *, #2086, .T. ) ;
#11388 = CARTESIAN_POINT ( 'NONE',  ( 66.44356964374999563, 71.84604660189820891, 3.696875000614517237 ) ) ;
#11389 = ORIENTED_EDGE ( 'NONE', *, *, #7308, .F. ) ;
#11390 = AXIS2_PLACEMENT_3D ( 'NONE', #4368, #7370, #6192 ) ;
#11391 = FACE_BOUND ( 'NONE', #2895, .T. ) ;
#11392 = AXIS2_PLACEMENT_3D ( 'NONE', #1036, #6008, #4190 ) ;
#11393 = CARTESIAN_POINT ( 'NONE',  ( 60.63303222545420823, 111.5086687406912347, 2.885734441871016021 ) ) ;
#11394 = ORIENTED_EDGE ( 'NONE', *, *, #10320, .F. ) ;
#11395 = EDGE_CURVE ( 'NONE', #4659, #6247, #10267, .T. ) ;
#11396 = CARTESIAN_POINT ( 'NONE',  ( 28.50000000000000355, 90.00000000000000000, 22.38477631085024555 ) ) ;
#11397 = CARTESIAN_POINT ( 'NONE',  ( 5.680405782532357506, 101.3717050593596127, 3.000000000000001776 ) ) ;
#11398 = ADVANCED_FACE ( 'NONE', ( #7604 ), #7540, .T. ) ;
#11399 = CARTESIAN_POINT ( 'NONE',  ( 50.72178482187499071, 117.2309300971526937, 3.359375000614517326 ) ) ;
#11400 = CYLINDRICAL_SURFACE ( 'NONE', #7901, 6.450000000000001066 ) ;
#11401 = AXIS2_PLACEMENT_3D ( 'NONE', #1270, #5262, #9251 ) ;
#11402 = PLANE ( 'NONE',  #3746 ) ;
#11403 = VECTOR ( 'NONE', #8092, 1000.000000000000227 ) ;
#11404 = CARTESIAN_POINT ( 'NONE',  ( 7.500000000000000000, 30.00000000000000000, 1.599999999999992095 ) ) ;
#11405 = FACE_OUTER_BOUND ( 'NONE', #3899, .T. ) ;
#11406 = CARTESIAN_POINT ( 'NONE',  ( 7.575919367743916943, 99.43635506061835372, 1.000000000000003109 ) ) ;
#11407 = DIRECTION ( 'NONE',  ( 0.000000000000000000, 0.000000000000000000, -1.000000000000000000 ) ) ;
#11408 = EDGE_CURVE ( 'NONE', #5251, #8056, #1517, .T. ) ;
#11409 = CIRCLE ( 'NONE', #5773, 28.99999999999999289 ) ;
#11410 = CYLINDRICAL_SURFACE ( 'NONE', #2528, 1.500000000000001332 ) ;
#11411 = DIRECTION ( 'NONE',  ( -1.000000000000000000, -0.000000000000000000, -0.000000000000000000 ) ) ;
#11412 = ORIENTED_EDGE ( 'NONE', *, *, #2957, .F. ) ;
#11413 = DIRECTION ( 'NONE',  ( 0.03100775193798452692, 0.9995191440486532741, 0.000000000000000000 ) ) ;
#11414 = CARTESIAN_POINT ( 'NONE',  ( 35.00000000000000000, 90.00000000000000000, -1.000000000000000000 ) ) ;
#11415 = ORIENTED_EDGE ( 'NONE', *, *, #6826, .T. ) ;
#11416 = AXIS2_PLACEMENT_3D ( 'NONE', #5521, #7490, #12334 ) ;
#11417 = CYLINDRICAL_SURFACE ( 'NONE', #12210, 32.70000000000000284 ) ;
#11418 = DIRECTION ( 'NONE',  ( -0.000000000000000000, -0.000000000000000000, 1.000000000000000000 ) ) ;
#11419 = LINE ( 'NONE', #11551, #3845 ) ;
#11420 = VERTEX_POINT ( 'NONE', #12771 ) ;
#11421 = CARTESIAN_POINT ( 'NONE',  ( 21.49999999999998579, 90.00000000000000000, -8.000000000000000000 ) ) ;
#11422 = CARTESIAN_POINT ( 'NONE',  ( 4.800000000000015810, 90.00000000000000000, 5.000000000000000000 ) ) ;
#11423 = EDGE_LOOP ( 'NONE', ( #8294, #11347, #10130, #9867, #5231, #10189 ) ) ;
#11424 = DIRECTION ( 'NONE',  ( 1.000000000000000000, 0.000000000000000000, 0.000000000000000000 ) ) ;
#11425 = CARTESIAN_POINT ( 'NONE',  ( -58.07179676972458537, 42.66025403784442460, -1.000000000000000000 ) ) ;
#11426 = VERTEX_POINT ( 'NONE', #7476 ) ;
#11427 = CIRCLE ( 'NONE', #4545, 1.500000000000001332 ) ;
#11428 = FACE_BOUND ( 'NONE', #10921, .T. ) ;
#11429 = VERTEX_POINT ( 'NONE', #4665 ) ;
#11430 = DIRECTION ( 'NONE',  ( -0.000000000000000000, -0.000000000000000000, -1.000000000000000000 ) ) ;
#11431 = PLANE ( 'NONE',  #4778 ) ;
#11432 = VERTEX_POINT ( 'NONE', #978 ) ;
#11433 = ADVANCED_FACE ( 'NONE', ( #6938 ), #7069, .F. ) ;
#11434 = EDGE_CURVE ( 'NONE', #865, #488, #9428, .T. ) ;
#11435 = PLANE ( 'NONE',  #8437 ) ;
#11436 = AXIS2_PLACEMENT_3D ( 'NONE', #6699, #1800, #10693 ) ;
#11437 = CARTESIAN_POINT ( 'NONE',  ( 1.269999999999999796, 3.490243377569956061E-16, -2.849999999999999645 ) ) ;
#11438 = EDGE_LOOP ( 'NONE', ( #12101, #3593, #4820, #2633 ) ) ;
#11439 = CARTESIAN_POINT ( 'NONE',  ( 2.179634403564814971, -5.614030811971695734, -0.8000000000000000444 ) ) ;
#11440 = CARTESIAN_POINT ( 'NONE',  ( 66.20000000000005969, 108.0133283987162685, 4.475000001229034297 ) ) ;
#11441 = VERTEX_POINT ( 'NONE', #5952 ) ;
#11442 = APPLICATION_CONTEXT ( 'automotive_design' ) ;
#11443 = LINE ( 'NONE', #4583, #8891 ) ;
#11444 = ORIENTED_EDGE ( 'NONE', *, *, #10021, .F. ) ;
#11445 = CYLINDRICAL_SURFACE ( 'NONE', #7974, 4.338286831716297698 ) ;
#11446 = VERTEX_POINT ( 'NONE', #9095 ) ;
#11447 = VECTOR ( 'NONE', #1377, 1000.000000000000000 ) ;
#11448 = CARTESIAN_POINT ( 'NONE',  ( 66.19999999999998863, 90.00000000000000000, 4.774999999999999467 ) ) ;
#11449 = CARTESIAN_POINT ( 'NONE',  ( 45.00000000000000000, 0.000000000000000000, 5.750000000000000888 ) ) ;
#11450 = UNCERTAINTY_MEASURE_WITH_UNIT (LENGTH_MEASURE( 1.000000000000000082E-05 ), #11723, 'distance_accuracy_value', 'NONE');
#11451 = VERTEX_POINT ( 'NONE', #2038 ) ;
#11452 = CARTESIAN_POINT ( 'NONE',  ( 3.556430356250028790, 71.84604660189818048, 3.996875000614517059 ) ) ;
#11453 = VERTEX_POINT ( 'NONE', #11051 ) ;
#11454 = EDGE_CURVE ( 'NONE', #10285, #10785, #11785, .T. ) ;
#11455 = CARTESIAN_POINT ( 'NONE',  ( 3.799999999999904787, 71.98667160128373155, 2.900000001229034563 ) ) ;
#11456 = VECTOR ( 'NONE', #5757, 1000.000000000000000 ) ;
#11457 = ORIENTED_EDGE ( 'NONE', *, *, #11951, .T. ) ;
#11458 = CARTESIAN_POINT ( 'NONE',  ( 3.556430356250015024, 90.00000000000000000, 4.803125000614516971 ) ) ;
#11459 = ORIENTED_EDGE ( 'NONE', *, *, #1964, .T. ) ;
#11460 = DIRECTION ( 'NONE',  ( 0.5000000000000049960, -0.8660254037844357100, 0.000000000000000000 ) ) ;
#11461 = DIRECTION ( 'NONE',  ( 0.000000000000000000, 0.000000000000000000, 1.000000000000000000 ) ) ;
#11462 = CARTESIAN_POINT ( 'NONE',  ( 35.00000000000000711, 53.69209320379639649, 3.171875000614517326 ) ) ;
#11463 = CARTESIAN_POINT ( 'NONE',  ( -9.666666666666657193, 61.36936462597000741, -1.000000000000000000 ) ) ;
#11465 = DIRECTION ( 'NONE',  ( -0.000000000000000000, 1.000000000000000000, -0.000000000000000000 ) ) ;
#11464 = AXIS2_PLACEMENT_3D ( 'NONE', #11186, #6215, #245 ) ;
#11466 = EDGE_CURVE ( 'NONE', #9137, #41, #4068, .T. ) ;
#11467 = CARTESIAN_POINT ( 'NONE',  ( 2.387319993259524598, -4.036502139894371233, -0.8000000000000000444 ) ) ;
#11468 = DIRECTION ( 'NONE',  ( 0.03100775193798453039, 0.9995191440486532741, -0.000000000000000000 ) ) ;
#11469 = EDGE_CURVE ( 'NONE', #9298, #5069, #2686, .T. ) ;
#11470 = CARTESIAN_POINT ( 'NONE',  ( 18.35999869903453430, 66.24638416994363865, 4.000000000000000000 ) ) ;
#11471 = DIRECTION ( 'NONE',  ( 1.000000000000000000, 0.000000000000000000, 0.000000000000000000 ) ) ;
#11472 = VECTOR ( 'NONE', #4158, 1000.000000000000000 ) ;
#11473 = DIRECTION ( 'NONE',  ( -0.5000000000000044409, 0.8660254037844360431, 0.000000000000000000 ) ) ;
#11474 = DIRECTION ( 'NONE',  ( -0.000000000000000000, 1.000000000000000000, 1.224646799147353207E-16 ) ) ;
#11475 = CARTESIAN_POINT ( 'NONE',  ( 50.59999999999999432, 117.0199925980744666, 3.612500001229034474 ) ) ;
#11476 = VERTEX_POINT ( 'NONE', #3018 ) ;
#11477 = CARTESIAN_POINT ( 'NONE',  ( 2.168404344971008868E-16, -0.5773502691896255090, 1.000000000000000000 ) ) ;
#11478 = DIRECTION ( 'NONE',  ( -0.5000000000000042188, 1.060575238724903710E-16, -0.8660254037844361541 ) ) ;
#11479 = ORIENTED_EDGE ( 'NONE', *, *, #1738, .T. ) ;
#11480 = PRODUCT ( 'base plate', 'base plate', '', ( #8633 ) ) ;
#11481 = FILL_AREA_STYLE_COLOUR ( '', #684 ) ;
#11482 = CIRCLE ( 'NONE', #186, 2.849999999999999201 ) ;
#11483 = EDGE_CURVE ( 'NONE', #5120, #7980, #6083, .T. ) ;
#11484 = DIRECTION ( 'NONE',  ( 0.000000000000000000, 0.000000000000000000, -1.000000000000000000 ) ) ;
#11485 = DIRECTION ( 'NONE',  ( -1.000000000000000000, 0.000000000000000000, 0.000000000000000000 ) ) ;
#11486 = CARTESIAN_POINT ( 'NONE',  ( 35.49992570027444572, 118.9956906159209069, 3.000000000000000888 ) ) ;
#11487 = EDGE_LOOP ( 'NONE', ( #10642, #2208, #1033, #5488 ) ) ;
#11488 = DIRECTION ( 'NONE',  ( -1.000000000000000000, 0.000000000000000000, 0.000000000000000000 ) ) ;
#11489 = DIRECTION ( 'NONE',  ( 0.000000000000000000, 0.000000000000000000, 1.000000000000000000 ) ) ;
#11490 = ORIENTED_EDGE ( 'NONE', *, *, #3056, .F. ) ;
#11491 = DIRECTION ( 'NONE',  ( 0.000000000000000000, -0.000000000000000000, -1.000000000000000000 ) ) ;
#11492 = VERTEX_POINT ( 'NONE', #850 ) ;
#11493 = FACE_OUTER_BOUND ( 'NONE', #8852, .T. ) ;
#11494 = VERTEX_POINT ( 'NONE', #10804 ) ;
#11495 = DIRECTION ( 'NONE',  ( -0.000000000000000000, 1.000000000000000000, -0.000000000000000000 ) ) ;
#11496 = DIRECTION ( 'NONE',  ( -0.000000000000000000, -0.000000000000000000, -1.000000000000000000 ) ) ;
#11497 = ORIENTED_EDGE ( 'NONE', *, *, #12347, .T. ) ;
#11498 = ADVANCED_FACE ( 'NONE', ( #7007 ), #3812, .F. ) ;
#11499 = VECTOR ( 'NONE', #671, 1000.000000000000114 ) ;
#11500 = ORIENTED_EDGE ( 'NONE', *, *, #7265, .T. ) ;
#11501 =( BOUNDED_CURVE ( )  B_SPLINE_CURVE ( 2, ( #754, #10831, #7956, #9787, #4945, #1935, #1874, #7760, #6710, #4756, #9849, #2006, #5006, #10702, #877, #1743, #8742, #4881, #12864, #12738, #2924, #10891, #11749, #6776, #4819, #10769, #815, #8805, #3909, #8215, #3317, #7163, #6309, #345, #3119, #5328, #1073, #277, #4295, #7297, #8021, #8152, #10042, #5065, #4230, #2333, #2204, #10299, #6246, #5134, #2271 ),
 .UNSPECIFIED., .F., .F. ) 
 B_SPLINE_CURVE_WITH_KNOTS ( ( 3, 2, 2, 2, 2, 2, 2, 2, 2, 2, 2, 2, 2, 2, 2, 2, 2, 2, 2, 2, 2, 2, 2, 2, 2, 3 ),
 ( 0.000000000000000000, 0.03333333333333333287, 0.06666666666666666574, 0.1000000000000000056, 0.1333333333333333315, 0.1666666666666666574, 0.2000000000000000111, 0.2333333333333333370, 0.2666666666666666630, 0.2999999999999999889, 0.3333333333333333148, 0.3666666666666666408, 0.4000000000000000222, 0.4333333333333333481, 0.4666666666666666741, 0.5000000000000000000, 0.5333333333333333259, 0.5666666666666666519, 0.5999999999999999778, 0.6333333333333333037, 0.6666666666666666297, 0.6999999999999999556, 0.7333333333333332815, 0.7666666666666667185, 0.8000000000000000444, 0.8259392087116486092 ),
 .UNSPECIFIED. ) 
 CURVE ( )  GEOMETRIC_REPRESENTATION_ITEM ( )  RATIONAL_B_SPLINE_CURVE ( ( 1.000000000000000000, 0.8660254037844387076, 1.000000000000000000, 0.8660254037844387076, 1.000000000000000000, 0.8660254037844387076, 1.000000000000000000, 0.8660254037844387076, 1.000000000000000000, 0.8660254037844387076, 1.000000000000000000, 0.8660254037844387076, 1.000000000000000000, 0.8660254037844387076, 1.000000000000000000, 0.8660254037844387076, 1.000000000000000000, 0.8660254037844387076, 1.000000000000000000, 0.8660254037844387076, 1.000000000000000000, 0.8660254037844387076, 1.000000000000000000, 0.8660254037844387076, 1.000000000000000000, 0.8660254037844387076, 1.000000000000000000, 0.8660254037844387076, 1.000000000000000000, 0.8660254037844387076, 1.000000000000000000, 0.8660254037844387076, 1.000000000000000000, 0.8660254037844387076, 1.000000000000000000, 0.8660254037844387076, 1.000000000000000000, 0.8660254037844387076, 1.000000000000000000, 0.8660254037844387076, 1.000000000000000000, 0.8660254037844387076, 1.000000000000000000, 0.8660254037844387076, 1.000000000000000000, 0.8660254037844387076, 1.000000000000000000, 0.8660254037844387076, 1.000000000000000000, 0.8957441496011714355, 0.9537471549766802781 ) ) 
 REPRESENTATION_ITEM ( '' )  );
#11502 = CARTESIAN_POINT ( 'NONE',  ( 46.89999999999997016, 90.00000000000000000, -10.00000000000000178 ) ) ;
#11503 = EDGE_LOOP ( 'NONE', ( #6482, #6937, #4399, #5096, #7891, #2029, #2272, #984 ) ) ;
#11504 = DIRECTION ( 'NONE',  ( -1.000000000000000000, 0.000000000000000000, 0.000000000000000000 ) ) ;
#11505 = APPLICATION_PROTOCOL_DEFINITION ( 'draft international standard', 'automotive_design', 1998, #12365 ) ;
#11506 = CARTESIAN_POINT ( 'NONE',  ( 35.00000000000000000, 126.0266567974326222, 4.100000001229034297 ) ) ;
#11507 = ORIENTED_EDGE ( 'NONE', *, *, #3660, .F. ) ;
#11508 = FILL_AREA_STYLE_COLOUR ( '', #9314 ) ;
#11509 = EDGE_CURVE ( 'NONE', #7217, #3039, #4978, .T. ) ;
#11510 = VERTEX_POINT ( 'NONE', #11849 ) ;
#11511 = EDGE_CURVE ( 'NONE', #4218, #3842, #10013, .T. ) ;
#11512 = CIRCLE ( 'NONE', #6280, 31.19999999999999218 ) ;
#11513 = DIRECTION ( 'NONE',  ( 0.000000000000000000, 0.000000000000000000, -1.000000000000000000 ) ) ;
#11514 = VERTEX_POINT ( 'NONE', #1043 ) ;
#11515 = CARTESIAN_POINT ( 'NONE',  ( -61.88397459621560870, 33.26313972081441506, 1.836970198721030427E-16 ) ) ;
#11516 = DIRECTION ( 'NONE',  ( 0.000000000000000000, 1.000000000000000000, 0.000000000000000000 ) ) ;
#11517 = EDGE_CURVE ( 'NONE', #4278, #9690, #12776, .T. ) ;
#11518 = VERTEX_POINT ( 'NONE', #9822 ) ;
#11519 = AXIS2_PLACEMENT_3D ( 'NONE', #3221, #7134, #3414 ) ;
#11520 = CARTESIAN_POINT ( 'NONE',  ( 50.60000000000001563, 62.98000740192552627, 4.362500001229034474 ) ) ;
#11521 = ORIENTED_EDGE ( 'NONE', *, *, #4324, .T. ) ;
#11522 = APPLICATION_CONTEXT ( 'automotive_design' ) ;
#11523 = CARTESIAN_POINT ( 'NONE',  ( 9.369499999999998607, 0.000000000000000000, 0.000000000000000000 ) ) ;
#11524 = ORIENTED_EDGE ( 'NONE', *, *, #5188, .T. ) ;
#11525 = CARTESIAN_POINT ( 'NONE',  ( 66.44356964374998142, 108.1539533981018053, 3.321875000614517237 ) ) ;
#11526 = EDGE_LOOP ( 'NONE', ( #894, #1165, #4461, #11367 ) ) ;
#11527 = LINE ( 'NONE', #9759, #5452 ) ;
#11528 = LINE ( 'NONE', #3626, #963 ) ;
#11529=STYLED_ITEM('',(#12981),#11875);
#11530 = CARTESIAN_POINT ( 'NONE',  ( 60.00000000000000000, -6.000000000000000000, -15.00000000000000355 ) ) ;
#11531 = EDGE_CURVE ( 'NONE', #2096, #4006, #5830, .T. ) ;
#11532 = DIRECTION ( 'NONE',  ( -1.000000000000000000, 0.000000000000000000, 0.000000000000000000 ) ) ;
#11533 = LINE ( 'NONE', #2649, #12309 ) ;
#11534 = CARTESIAN_POINT ( 'NONE',  ( -0.1038759689922479496, -3.348389132562988646, -0.8000000000000000444 ) ) ;
#11535 = CARTESIAN_POINT ( 'NONE',  ( 3.800000000000015365, 90.00000000000000000, 4.831250000614517148 ) ) ;
#11536 = CARTESIAN_POINT ( 'NONE',  ( 35.75000000000000711, 92.49999999999998579, 4.800000000000000711 ) ) ;
#11537 = VECTOR ( 'NONE', #1323, 1000.000000000000000 ) ;
#11538 = CARTESIAN_POINT ( 'NONE',  ( -57.99999999999999289, 2.000000000000000000, -8.000000000000003553 ) ) ;
#11539 = EDGE_CURVE ( 'NONE', #8374, #9930, #4854, .T. ) ;
#11540 = CARTESIAN_POINT ( 'NONE',  ( 25.00000000000000355, -5.000000000000000000, 7.250000000000000888 ) ) ;
#11541 = CARTESIAN_POINT ( 'NONE',  ( -3.666666666666651420, 62.52406516434930239, 2.999999999999902300 ) ) ;
#11542 = ORIENTED_EDGE ( 'NONE', *, *, #7323, .T. ) ;
#11543 = CARTESIAN_POINT ( 'NONE',  ( 66.19999999999998863, 90.00000000000000000, 3.425000000000000266 ) ) ;
#11544 = LINE ( 'NONE', #1607, #10606 ) ;
#11545 = ORIENTED_EDGE ( 'NONE', *, *, #5579, .F. ) ;
#11546 = EDGE_CURVE ( 'NONE', #12580, #8640, #3881, .T. ) ;
#11547 = PRESENTATION_STYLE_ASSIGNMENT (( #7560 ) ) ;
#11548 = VECTOR ( 'NONE', #1688, 1000.000000000000227 ) ;
#11549 = CARTESIAN_POINT ( 'NONE',  ( 22.99999999999998579, 90.00000000000000000, -8.000000000000000000 ) ) ;
#11550 = PLANE ( 'NONE',  #1373 ) ;
#11551 = CARTESIAN_POINT ( 'NONE',  ( 3.678215178125014972, 90.00000000000000000, 4.929687500307258219 ) ) ;
#11552 = ORIENTED_EDGE ( 'NONE', *, *, #9974, .F. ) ;
#11553 = DIRECTION ( 'NONE',  ( 0.000000000000000000, -0.000000000000000000, 1.000000000000000000 ) ) ;
#11554 = CARTESIAN_POINT ( 'NONE',  ( -3.666666666666661634, 64.83346624110779999, -1.000000000000000666 ) ) ;
#11555 = VERTEX_POINT ( 'NONE', #2898 ) ;
#11556 = CARTESIAN_POINT ( 'NONE',  ( -61.13397459621560159, 31.96410161513775350, 0.000000000000000000 ) ) ;
#11557 = DIRECTION ( 'NONE',  ( -1.000000000000000000, 0.000000000000000000, 0.000000000000000000 ) ) ;
#11558 = ORIENTED_EDGE ( 'NONE', *, *, #7675, .F. ) ;
#11559 = ADVANCED_FACE ( 'NONE', ( #910 ), #5035, .F. ) ;
#11560 = DIRECTION ( 'NONE',  ( 0.000000000000000000, -1.000000000000000000, 0.000000000000000000 ) ) ;
#11561 = ORIENTED_EDGE ( 'NONE', *, *, #4252, .F. ) ;
#11562 = VECTOR ( 'NONE', #5049, 1000.000000000000000 ) ;
#11563 = EDGE_CURVE ( 'NONE', #12318, #1018, #8998, .T. ) ;
#11564 = DIRECTION ( 'NONE',  ( -0.000000000000000000, 0.5000000000000003331, -0.8660254037844383745 ) ) ;
#11565 = CYLINDRICAL_SURFACE ( 'NONE', #8950, 2.849999999999999645 ) ;
#11566 = STYLED_ITEM ( 'NONE', ( #11386 ), #5287 ) ;
#11567 = CARTESIAN_POINT ( 'NONE',  ( -0.1038759689922479496, -3.348389132562988646, 0.000000000000000000 ) ) ;
#11568 = LINE ( 'NONE', #1560, #4686 ) ;
#11569 = CYLINDRICAL_SURFACE ( 'NONE', #10964, 1.500000000000001332 ) ;
#11570 = ORIENTED_EDGE ( 'NONE', *, *, #596, .T. ) ;
#11571 = VECTOR ( 'NONE', #1819, 1000.000000000000114 ) ;
#11572 = CARTESIAN_POINT ( 'NONE',  ( 9.999999999999994671, 30.00000000000000000, 2.500000000000000444 ) ) ;
#11573 = CARTESIAN_POINT ( 'NONE',  ( 50.59999999999999432, 117.0199925980744666, 4.062500001229034652 ) ) ;
#11574 = VERTEX_POINT ( 'NONE', #2958 ) ;
#11575 = ORIENTED_EDGE ( 'NONE', *, *, #9946, .F. ) ;
#11576 = EDGE_CURVE ( 'NONE', #11510, #9327, #11725, .T. ) ;
#11577 = ORIENTED_EDGE ( 'NONE', *, *, #4317, .T. ) ;
#11578 = CYLINDRICAL_SURFACE ( 'NONE', #9636, 1.499999999999999556 ) ;
#11579 = ORIENTED_EDGE ( 'NONE', *, *, #500, .T. ) ;
#11580 = CARTESIAN_POINT ( 'NONE',  ( 18.38891503675719008, 63.42664337523432039, 3.000000000000000888 ) ) ;
#11581 = LINE ( 'NONE', #6540, #12708 ) ;
#11582 = VECTOR ( 'NONE', #4612, 1000.000000000000114 ) ;
#11583 = AXIS2_PLACEMENT_3D ( 'NONE', #11679, #12603, #748 ) ;
#11585 = EDGE_CURVE ( 'NONE', #6465, #7786, #6297, .T. ) ;
#11584 = EDGE_LOOP ( 'NONE', ( #11375, #1553, #7298, #4565, #278 ) ) ;
#11586 = CARTESIAN_POINT ( 'NONE',  ( -6.666666666666660745, 0.000000000000000000, 0.000000000000000000 ) ) ;
#11587 = VERTEX_POINT ( 'NONE', #7201 ) ;
#11588 = CARTESIAN_POINT ( 'NONE',  ( 35.00000000000000000, 126.0266567974326222, 3.200000001229034385 ) ) ;
#11589 = ORIENTED_EDGE ( 'NONE', *, *, #5470, .F. ) ;
#11590 = CIRCLE ( 'NONE', #6144, 1.219500000000000028 ) ;
#11591 = CARTESIAN_POINT ( 'NONE',  ( 19.27821517812503060, 62.76906990284727783, 3.584375000614516971 ) ) ;
#11592 = PRODUCT_DEFINITION_SHAPE ( 'NONE', 'NONE',  #11777 ) ;
#11593 = ORIENTED_EDGE ( 'NONE', *, *, #11009, .T. ) ;
#11594 = CIRCLE ( 'NONE', #5942, 28.99999999999999289 ) ;
#11595 = CARTESIAN_POINT ( 'NONE',  ( -60.00000000000000000, -6.000000000000000000, 14.99999999999999645 ) ) ;
#11596 = CARTESIAN_POINT ( 'NONE',  ( 52.22659979626835991, 65.43896868087158225, -3.000000000000000000 ) ) ;
#11597 = LINE ( 'NONE', #7607, #8820 ) ;
#11598 = CARTESIAN_POINT ( 'NONE',  ( -31.49999999999998579, 79.07477288111861924, 1.000000000000000000 ) ) ;
#11599 = VECTOR ( 'NONE', #4627, 1000.000000000000114 ) ;
#11600 = DIRECTION ( 'NONE',  ( -0.000000000000000000, -1.000000000000000000, -0.000000000000000000 ) ) ;
#11601 = ADVANCED_FACE ( 'NONE', ( #11189 ), #6407, .T. ) ;
#11602 = EDGE_CURVE ( 'NONE', #1292, #8153, #1177, .T. ) ;
#11603 = AXIS2_PLACEMENT_3D ( 'NONE', #9084, #3281, #7258 ) ;
#11604 = CARTESIAN_POINT ( 'NONE',  ( 1.040000000000000036, -0.5773502691896253980, -1.000000000000000000 ) ) ;
#11605 = CARTESIAN_POINT ( 'NONE',  ( 45.00000000000000000, 0.000000000000000000, 7.349999999999997868 ) ) ;
#11606 = CARTESIAN_POINT ( 'NONE',  ( 35.75000000000000711, 92.49999999999998579, -9.802775637731997449 ) ) ;
#11607 = CARTESIAN_POINT ( 'NONE',  ( 7.573869524628007888, 99.43702109502098097, 4.000000000000000000 ) ) ;
#11608 = CARTESIAN_POINT ( 'NONE',  ( 3.800000000000015810, 108.0133283987162969, 3.612500000000000711 ) ) ;
#11609 = AXIS2_PLACEMENT_3D ( 'NONE', #10827, #4942, #11746 ) ;
#11610 = DIRECTION ( 'NONE',  ( -0.000000000000000000, -0.000000000000000000, 1.000000000000000000 ) ) ;
#11611 = ORIENTED_EDGE ( 'NONE', *, *, #10440, .F. ) ;
#11612 = AXIS2_PLACEMENT_3D ( 'NONE', #12778, #4798, #10377 ) ;
#11613 = CARTESIAN_POINT ( 'NONE',  ( 3.800000000000025135, 71.98667160128366049, 4.587500000000001243 ) ) ;
#11614 = CARTESIAN_POINT ( 'NONE',  ( -60.00000000000000000, 30.00000000000000000, 2.500000000000000000 ) ) ;
#11615 = VERTEX_POINT ( 'NONE', #10140 ) ;
#11616 = CARTESIAN_POINT ( 'NONE',  ( 35.75000000000000711, 92.49999999999998579, -3.799999999999999378 ) ) ;
#11617 = AXIS2_PLACEMENT_3D ( 'NONE', #5716, #8976, #12846 ) ;
#11618 = FACE_OUTER_BOUND ( 'NONE', #6082, .T. ) ;
#11619 = VERTEX_POINT ( 'NONE', #3354 ) ;
#11620 = DIRECTION ( 'NONE',  ( 0.8660254037844365982, 0.5000000000000036637, 0.000000000000000000 ) ) ;
#11621 = EDGE_CURVE ( 'NONE', #112, #261, #10404, .T. ) ;
#11622 = CARTESIAN_POINT ( 'NONE',  ( 50.00000000000000000, 2.000000000000000000, -10.00000000000000000 ) ) ;
#11623 = DIRECTION ( 'NONE',  ( -0.000000000000000000, -0.4999999999999999445, -0.8660254037844387076 ) ) ;
#11624 = LINE ( 'NONE', #12675, #115 ) ;
#11625 = ORIENTED_EDGE ( 'NONE', *, *, #3895, .F. ) ;
#11626 = DIRECTION ( 'NONE',  ( -0.000000000000000000, -1.000000000000000000, -0.000000000000000000 ) ) ;
#11627 = ORIENTED_EDGE ( 'NONE', *, *, #3010, .T. ) ;
#11628 = VECTOR ( 'NONE', #7425, 1000.000000000000000 ) ;
#11629 = CARTESIAN_POINT ( 'NONE',  ( 21.49999999999998579, 90.00000000000000000, -8.000000000000000000 ) ) ;
#11630 = CARTESIAN_POINT ( 'NONE',  ( 34.25000000000000000, 92.49999999999998579, 6.000000000000000000 ) ) ;
#11631 = LINE ( 'NONE', #6654, #2894 ) ;
#11632 = EDGE_CURVE ( 'NONE', #7921, #6585, #8801, .T. ) ;
#11633 = EDGE_CURVE ( 'NONE', #4210, #9895, #5168, .T. ) ;
#11634 = VERTEX_POINT ( 'NONE', #5361 ) ;
#11635 = DIRECTION ( 'NONE',  ( -0.000000000000000000, 1.000000000000000000, -0.000000000000000000 ) ) ;
#11636 = VERTEX_POINT ( 'NONE', #1375 ) ;
#11637 = CARTESIAN_POINT ( 'NONE',  ( 30.00000000000000711, 0.000000000000000000, 10.00000000000000000 ) ) ;
#11638 = EDGE_CURVE ( 'NONE', #8631, #3957, #7267, .T. ) ;
#11639 = DIRECTION ( 'NONE',  ( 0.4999999999999985012, -0.8660254037844394848, -0.000000000000000000 ) ) ;
#11640 = AXIS2_PLACEMENT_3D ( 'NONE', #9979, #3057, #8807 ) ;
#11641 = VERTEX_POINT ( 'NONE', #11314 ) ;
#11642 = DIRECTION ( 'NONE',  ( -1.000000000000000000, 0.000000000000000000, 0.000000000000000000 ) ) ;
#11643 = ORIENTED_EDGE ( 'NONE', *, *, #5751, .T. ) ;
#11644 = ORIENTED_EDGE ( 'NONE', *, *, #1100, .F. ) ;
#11645 = CARTESIAN_POINT ( 'NONE',  ( 13.83140072625826811, 66.88874552888529479, 3.000000000000000888 ) ) ;
#11646 = CARTESIAN_POINT ( 'NONE',  ( 19.40000000000002700, 62.98000740192551206, 3.275000000000000355 ) ) ;
#11647 = VECTOR ( 'NONE', #9709, 1000.000000000000114 ) ;
#11648 = ADVANCED_FACE ( 'NONE', ( #9358 ), #12106, .F. ) ;
#11649 = EDGE_LOOP ( 'NONE', ( #3805, #10321, #9774, #5683 ) ) ;
#11650 = CARTESIAN_POINT ( 'NONE',  ( -0.9999999999999997780, -4.273461295629625845, -0.8000000000000000444 ) ) ;
#11651 = ORIENTED_EDGE ( 'NONE', *, *, #2803, .F. ) ;
#11652 = CARTESIAN_POINT ( 'NONE',  ( 3.800000000000015810, 108.0133283987162969, 3.275000001229034563 ) ) ;
#11653 = VERTEX_POINT ( 'NONE', #10340 ) ;
#11654 = CARTESIAN_POINT ( 'NONE',  ( 66.44356964374998142, 108.1539533981018053, 3.715625000614517948 ) ) ;
#11655 = ORIENTED_EDGE ( 'NONE', *, *, #2856, .F. ) ;
#11656 = AXIS2_PLACEMENT_3D ( 'NONE', #5429, #447, #583 ) ;
#11657 = CARTESIAN_POINT ( 'NONE',  ( 35.00000000000000000, 126.0266567974326222, 3.987500000000000266 ) ) ;
#11658 = CARTESIAN_POINT ( 'NONE',  ( 20.00000000000000355, 0.000000000000000000, 1.500000000000000444 ) ) ;
#11659 = CARTESIAN_POINT ( 'NONE',  ( -48.33333333333332860, 0.000000000000000000, -1.599999999999998979 ) ) ;
#11660 = CARTESIAN_POINT ( 'NONE',  ( 60.63303222545420823, 111.5086687406912347, 2.829484441871016109 ) ) ;
#11661 = DIRECTION ( 'NONE',  ( 0.000000000000000000, 0.000000000000000000, 1.000000000000000000 ) ) ;
#11662 = AXIS2_PLACEMENT_3D ( 'NONE', #10245, #5270, #12078 ) ;
#11663 = EDGE_CURVE ( 'NONE', #8770, #255, #1245, .T. ) ;
#11664 = VECTOR ( 'NONE', #9542, 1000.000000000000000 ) ;
#11665 = CARTESIAN_POINT ( 'NONE',  ( 3.800000000000015365, 90.00000000000000000, 3.762500001229034385 ) ) ;
#11666 = DIRECTION ( 'NONE',  ( 0.5000000000000005551, -0.8660254037844383745, 0.000000000000000000 ) ) ;
#11667 = DIRECTION ( 'NONE',  ( -0.000000000000000000, -1.000000000000000000, -0.000000000000000000 ) ) ;
#11668 = DIRECTION ( 'NONE',  ( -1.000000000000000000, 0.000000000000000000, 0.000000000000000000 ) ) ;
#11669 = CARTESIAN_POINT ( 'NONE',  ( 35.00000000000000000, 126.0266567974326222, 3.537499999999999645 ) ) ;
#11670 = CARTESIAN_POINT ( 'NONE',  ( 35.00000000000000000, 126.3079067962035822, 3.396875000614517415 ) ) ;
#11672 = ADVANCED_FACE ( 'NONE', ( #10271 ), #11379, .T. ) ;
#11671 = ORIENTED_EDGE ( 'NONE', *, *, #10676, .F. ) ;
#11673 = AXIS2_PLACEMENT_3D ( 'NONE', #10163, #10094, #5124 ) ;
#11674 = ADVANCED_FACE ( 'NONE', ( #4264 ), #4199, .F. ) ;
#11675 = CARTESIAN_POINT ( 'NONE',  ( 3.800000000000015365, 90.00000000000000000, 3.200000000000000178 ) ) ;
#11676 = DIRECTION ( 'NONE',  ( 0.000000000000000000, 0.000000000000000000, -1.000000000000000000 ) ) ;
#11677 = ORIENTED_EDGE ( 'NONE', *, *, #34, .F. ) ;
#11678 = VECTOR ( 'NONE', #5962, 1000.000000000000000 ) ;
#11679 = CARTESIAN_POINT ( 'NONE',  ( 3.556430356250015024, 90.00000000000000000, 4.831250000614517148 ) ) ;
#11680 = FACE_BOUND ( 'NONE', #3466, .T. ) ;
#11681 = AXIS2_PLACEMENT_3D ( 'NONE', #6881, #2775, #1722 ) ;
#11682 = CARTESIAN_POINT ( 'NONE',  ( 1.040000000000000036, -0.5773502691896256200, -1.000000000000000000 ) ) ;
#11683 = CARTESIAN_POINT ( 'NONE',  ( 3.556430356250014579, 108.1539533981018053, 3.865625000614517415 ) ) ;
#11684 = CARTESIAN_POINT ( 'NONE',  ( -1.436050757534458100, -5.516136167806656943, 0.000000000000000000 ) ) ;
#11685 = DIRECTION ( 'NONE',  ( -1.000000000000000000, -5.551115123125781124E-15, 0.000000000000000000 ) ) ;
#11686 = ORIENTED_EDGE ( 'NONE', *, *, #4700, .T. ) ;
#11687 = CARTESIAN_POINT ( 'NONE',  ( 33.50000000000000711, 67.79999999999999716, 6.000000000000000000 ) ) ;
#11688 = VERTEX_POINT ( 'NONE', #2365 ) ;
#11689 = CYLINDRICAL_SURFACE ( 'NONE', #8828, 1.499999999999998668 ) ;
#11690 = CARTESIAN_POINT ( 'NONE',  ( -0.1038759689922479496, -3.348389132562988646, -0.8000000000000000444 ) ) ;
#11691 = EDGE_CURVE ( 'NONE', #9467, #7727, #4391, .T. ) ;
#11692 = SHAPE_REPRESENTATION ( 'wheel support and navigator', ( #5704 ), #11354 ) ;
#11693 = DIRECTION ( 'NONE',  ( -1.000000000000000000, 0.000000000000000000, 0.000000000000000000 ) ) ;
#11694 = PRODUCT_DEFINITION_SHAPE ( 'NONE', 'NONE',  #12969 ) ;
#11695 = DIRECTION ( 'NONE',  ( 0.000000000000000000, 0.000000000000000000, -1.000000000000000000 ) ) ;
#11697 = CARTESIAN_POINT ( 'NONE',  ( 34.50001867552290946, 118.9978264099154615, 4.000000000000000000 ) ) ;
#11696 = AXIS2_PLACEMENT_3D ( 'NONE', #3923, #5872, #8760 ) ;
#11698 = ORIENTED_EDGE ( 'NONE', *, *, #1510, .T. ) ;
#11699 = LINE ( 'NONE', #11572, #4078 ) ;
#11700 = CONTEXT_DEPENDENT_SHAPE_REPRESENTATION ( #5598, #7948 ) ;
#11701 = LINE ( 'NONE', #769, #6896 ) ;
#11702 = EDGE_LOOP ( 'NONE', ( #2825, #2376 ) ) ;
#11703 = DIRECTION ( 'NONE',  ( -0.000000000000000000, -0.000000000000000000, 1.000000000000000000 ) ) ;
#11704 = ORIENTED_EDGE ( 'NONE', *, *, #3180, .T. ) ;
#11705 = EDGE_CURVE ( 'NONE', #11587, #12162, #11116, .T. ) ;
#11706 = CARTESIAN_POINT ( 'NONE',  ( 64.31840935109022439, 100.6710296186405742, 2.661976390793298286 ) ) ;
#11707 = VERTEX_POINT ( 'NONE', #5300 ) ;
#11708 = CARTESIAN_POINT ( 'NONE',  ( 5.604701438244304335, 78.90188256379346399, 2.999999999999998668 ) ) ;
#11709 = VECTOR ( 'NONE', #3652, 1000.000000000000000 ) ;
#11710 = FACE_OUTER_BOUND ( 'NONE', #2847, .T. ) ;
#11711 = AXIS2_PLACEMENT_3D ( 'NONE', #8755, #1820, #9669 ) ;
#11712 = ADVANCED_FACE ( 'NONE', ( #1306 ), #9292, .T. ) ;
#11713 = EDGE_LOOP ( 'NONE', ( #3171, #6953, #7536, #8995 ) ) ;
#11714 = EDGE_LOOP ( 'NONE', ( #11387, #9139, #3491, #2098, #2703 ) ) ;
#11715 = FACE_BOUND ( 'NONE', #1684, .T. ) ;
#11716 = ORIENTED_EDGE ( 'NONE', *, *, #1861, .F. ) ;
#11717 = VECTOR ( 'NONE', #6954, 1000.000000000000000 ) ;
#11718 = PLANE ( 'NONE',  #10719 ) ;
#11719 = ORIENTED_EDGE ( 'NONE', *, *, #994, .T. ) ;
#11720 = DIRECTION ( 'NONE',  ( 0.000000000000000000, 0.000000000000000000, 1.000000000000000000 ) ) ;
#11721 = CARTESIAN_POINT ( 'NONE',  ( 3.800000000000015365, 90.00000000000000000, 4.100000000000000533 ) ) ;
#11722 = ADVANCED_FACE ( 'NONE', ( #10535 ), #11578, .F. ) ;
#11723 =( LENGTH_UNIT ( ) NAMED_UNIT ( * ) SI_UNIT ( .MILLI., .METRE. ) );
#11724 = CARTESIAN_POINT ( 'NONE',  ( 3.800000000000025135, 71.98667160128366049, 4.250000001229034652 ) ) ;
#11725 = CIRCLE ( 'NONE', #6499, 0.5999999999999998668 ) ;
#11726 = CARTESIAN_POINT ( 'NONE',  ( -60.00000000000000000, -6.000000000000000000, -15.00000000000000355 ) ) ;
#11727 = CARTESIAN_POINT ( 'NONE',  ( 6.499999999999999112, 70.70319397786906279, -1.000000000000000000 ) ) ;
#11728 = CARTESIAN_POINT ( 'NONE',  ( -65.00000000000004263, 38.66025403784436065, 3.000000000000000000 ) ) ;
#11729 = DIRECTION ( 'NONE',  ( 1.000000000000000000, 0.000000000000000000, 0.000000000000000000 ) ) ;
#11730 = DIRECTION ( 'NONE',  ( 1.000000000000000000, -0.000000000000000000, -0.000000000000000000 ) ) ;
#11731 =( GEOMETRIC_REPRESENTATION_CONTEXT ( 3 ) GLOBAL_UNCERTAINTY_ASSIGNED_CONTEXT ( ( #2696 ) ) GLOBAL_UNIT_ASSIGNED_CONTEXT ( ( #163, #8795, #10630 ) ) REPRESENTATION_CONTEXT ( 'NONE', 'WORKASPACE' ) );
#11732 = DIRECTION ( 'NONE',  ( 0.000000000000000000, 0.000000000000000000, 1.000000000000000000 ) ) ;
#11733 = CARTESIAN_POINT ( 'NONE',  ( 66.44356964374999563, 90.00000000000000000, 3.284375000614517148 ) ) ;
#11734 = ORIENTED_EDGE ( 'NONE', *, *, #11956, .T. ) ;
#11735 = EDGE_CURVE ( 'NONE', #1744, #85, #1703, .T. ) ;
#11736 = CARTESIAN_POINT ( 'NONE',  ( 3.800000000000015365, 108.0133283987163111, 4.962499999999999467 ) ) ;
#11737 = CARTESIAN_POINT ( 'NONE',  ( 7.650000000000000355, 0.000000000000000000, 0.000000000000000000 ) ) ;
#11738 = EDGE_LOOP ( 'NONE', ( #10595, #9818 ) ) ;
#11739 = FILL_AREA_STYLE ('',( #12729 ) ) ;
#11740 = VECTOR ( 'NONE', #248, 999.9999999999998863 ) ;
#11741 = LINE ( 'NONE', #12857, #2401 ) ;
#11742 = EDGE_CURVE ( 'NONE', #6062, #12512, #9485, .T. ) ;
#11743 = DIRECTION ( 'NONE',  ( -1.000000000000000000, 0.000000000000000000, 0.000000000000000000 ) ) ;
#11744 = EDGE_CURVE ( 'NONE', #6635, #716, #709, .T. ) ;
#11745 = MANIFOLD_SOLID_BREP ( 'M3 Clearance Hole1', #699 ) ;
#11746 = DIRECTION ( 'NONE',  ( 1.000000000000000000, 0.000000000000000000, 0.000000000000000000 ) ) ;
#11747 = CARTESIAN_POINT ( 'NONE',  ( 3.556430356250028790, 71.84604660189818048, 3.040625000614517681 ) ) ;
#11748 = CARTESIAN_POINT ( 'NONE',  ( -60.00000000000000000, 30.00000000000000000, 1.000000000000005551 ) ) ;
#11749 = CARTESIAN_POINT ( 'NONE',  ( 19.27821517812503060, 62.76906990284727783, 4.034375000614517148 ) ) ;
#11750 = VERTEX_POINT ( 'NONE', #7528 ) ;
#11751 = VECTOR ( 'NONE', #9810, 1000.000000000000000 ) ;
#11752 = FACE_BOUND ( 'NONE', #6286, .T. ) ;
#11753 = ORIENTED_EDGE ( 'NONE', *, *, #8141, .F. ) ;
#11754 = ADVANCED_FACE ( 'NONE', ( #9555 ), #10468, .T. ) ;
#11755 = CARTESIAN_POINT ( 'NONE',  ( 31.99902028769960438, 88.51116798584881451, -3.800000000000000266 ) ) ;
#11756 = FACE_OUTER_BOUND ( 'NONE', #6163, .T. ) ;
#11757 = LINE ( 'NONE', #1818, #5292 ) ;
#11758 = CARTESIAN_POINT ( 'NONE',  ( 35.00000000000000000, 90.00000000000000000, -10.00000000000000000 ) ) ;
#11759 = ADVANCED_FACE ( 'NONE', ( #12695 ), #11445, .T. ) ;
#11760 =( GEOMETRIC_REPRESENTATION_CONTEXT ( 3 ) GLOBAL_UNCERTAINTY_ASSIGNED_CONTEXT ( ( #10540 ) ) GLOBAL_UNIT_ASSIGNED_CONTEXT ( ( #2138, #7689, #10374 ) ) REPRESENTATION_CONTEXT ( 'NONE', 'WORKASPACE' ) );
#11761 = FACE_OUTER_BOUND ( 'NONE', #5759, .T. ) ;
#11762 = VERTEX_POINT ( 'NONE', #1763 ) ;
#11763 = CARTESIAN_POINT ( 'NONE',  ( 0.000000000000000000, 0.4117131682837005258, -0.8000000000000000444 ) ) ;
#11764 = FACE_OUTER_BOUND ( 'NONE', #4166, .T. ) ;
#11765 = ORIENTED_EDGE ( 'NONE', *, *, #1891, .F. ) ;
#11766 = CIRCLE ( 'NONE', #7385, 1.500000000000001332 ) ;
#11767 =( NAMED_UNIT ( * ) SI_UNIT ( $, .STERADIAN. ) SOLID_ANGLE_UNIT ( ) );
#11768 = ORIENTED_EDGE ( 'NONE', *, *, #1687, .T. ) ;
#11769 = DIRECTION ( 'NONE',  ( 0.000000000000000000, 0.000000000000000000, 1.000000000000000000 ) ) ;
#11770 = ORIENTED_EDGE ( 'NONE', *, *, #8064, .T. ) ;
#11771 = DIRECTION ( 'NONE',  ( -0.000000000000000000, -0.000000000000000000, 1.000000000000000000 ) ) ;
#11772 =( GEOMETRIC_REPRESENTATION_CONTEXT ( 3 ) GLOBAL_UNCERTAINTY_ASSIGNED_CONTEXT ( ( #7659 ) ) GLOBAL_UNIT_ASSIGNED_CONTEXT ( ( #2044, #5173, #9161 ) ) REPRESENTATION_CONTEXT ( 'NONE', 'WORKASPACE' ) );
#11773 = CARTESIAN_POINT ( 'NONE',  ( 34.25000000000000000, 92.49999999999998579, -9.802775637731997449 ) ) ;
#11774 = VECTOR ( 'NONE', #3981, 1000.000000000000000 ) ;
#11775 = VERTEX_POINT ( 'NONE', #9420 ) ;
#11776 = CARTESIAN_POINT ( 'NONE',  ( 3.033375984251971413, -3.035766082959412415E-15, 0.000000000000000000 ) ) ;
#11777 = PRODUCT_DEFINITION ( 'UNKNOWN', '', #11992, #1359 ) ;
#11778 = VERTEX_POINT ( 'NONE', #7718 ) ;
#11779 = CARTESIAN_POINT ( 'NONE',  ( 31.86464806177570352, 88.44450386581220869, -3.799999999999999378 ) ) ;
#11780 = AXIS2_PLACEMENT_3D ( 'NONE', #6210, #3148, #1301 ) ;
#11781 = VERTEX_POINT ( 'NONE', #11706 ) ;
#11782 = CARTESIAN_POINT ( 'NONE',  ( 3.556430356250028790, 71.84604660189818048, 3.940625000614518036 ) ) ;
#11783 = EDGE_CURVE ( 'NONE', #3363, #5372, #1570, .T. ) ;
#11784 = ORIENTED_EDGE ( 'NONE', *, *, #3180, .F. ) ;
#11785 = LINE ( 'NONE', #4916, #8180 ) ;
#11786 = AXIS2_PLACEMENT_3D ( 'NONE', #8927, #7817, #4940 ) ;
#11787 = CARTESIAN_POINT ( 'NONE',  ( 3.068288344391240763, -2.655262421758693314, -0.8000000000000000444 ) ) ;
#11788 = AXIS2_PLACEMENT_3D ( 'NONE', #11011, #11810, #11873 ) ;
#11789 = SURFACE_STYLE_FILL_AREA ( #10739 ) ;
#11790 = CARTESIAN_POINT ( 'NONE',  ( 19.40000000000000924, 117.0199925980744666, 4.587500001229034119 ) ) ;
#11791 = MANIFOLD_SOLID_BREP ( 'M3 Clearance Hole2', #6755 ) ;
#11792 = DIRECTION ( 'NONE',  ( -0.000000000000000000, -0.000000000000000000, -1.000000000000000000 ) ) ;
#11793 = DIRECTION ( 'NONE',  ( -0.000000000000000000, -0.000000000000000000, -1.000000000000000000 ) ) ;
#11794 = FACE_OUTER_BOUND ( 'NONE', #7244, .T. ) ;
#11795 = VECTOR ( 'NONE', #5355, 1000.000000000000000 ) ;
#11796 = EDGE_CURVE ( 'NONE', #3150, #8914, #9644, .T. ) ;
#11797 = CARTESIAN_POINT ( 'NONE',  ( 51.63935276957964504, 66.24642824321904300, 4.000000000000000000 ) ) ;
#11798 = CARTESIAN_POINT ( 'NONE',  ( 0.000000000000000000, 0.000000000000000000, 0.000000000000000000 ) ) ;
#11799 = CIRCLE ( 'NONE', #6366, 10.00000000000000178 ) ;
#11800 = CARTESIAN_POINT ( 'NONE',  ( 35.00000000000000000, 90.00000000000000000, -3.000000000000000888 ) ) ;
#11801 = ADVANCED_FACE ( 'NONE', ( #10970 ), #2883, .T. ) ;
#11802 = VERTEX_POINT ( 'NONE', #6001 ) ;
#11803 = CARTESIAN_POINT ( 'NONE',  ( 66.20000000000008811, 108.0133283987162542, 3.462499999999999467 ) ) ;
#11804 = CARTESIAN_POINT ( 'NONE',  ( 19.27821517812500574, 117.2309300971526937, 3.434375000614517059 ) ) ;
#11805 = EDGE_LOOP ( 'NONE', ( #11363, #2617, #3893, #11988 ) ) ;
#11806 = CARTESIAN_POINT ( 'NONE',  ( 19.40000000000002700, 62.98000740192551206, 4.625000000000000000 ) ) ;
#11807 = CARTESIAN_POINT ( 'NONE',  ( 35.00000000000000000, 90.00000000000000000, 4.000000000000000000 ) ) ;
#11808 = EDGE_LOOP ( 'NONE', ( #2090, #9582, #5305, #8110, #8426 ) ) ;
#11809 = AXIS2_PLACEMENT_3D ( 'NONE', #10524, #10330, #12359 ) ;
#11810 = DIRECTION ( 'NONE',  ( -0.000000000000000000, -1.000000000000000000, -0.000000000000000000 ) ) ;
#11811 = ADVANCED_FACE ( 'NONE', ( #4901 ), #2818, .T. ) ;
#11812 = FACE_BOUND ( 'NONE', #12415, .T. ) ;
#11813 = CIRCLE ( 'NONE', #11173, 1.500000000000001332 ) ;
#11814 = CARTESIAN_POINT ( 'NONE',  ( 1.000000000000000000, -4.273461295629625845, 0.000000000000000000 ) ) ;
#11815 = CARTESIAN_POINT ( 'NONE',  ( 35.00000000000000711, 53.69209320379639649, 3.115625000614517415 ) ) ;
#11816 = VECTOR ( 'NONE', #3478, 1000.000000000000114 ) ;
#11817 = LINE ( 'NONE', #9848, #5225 ) ;
#11818 = DIRECTION ( 'NONE',  ( 0.000000000000000000, 0.000000000000000000, 1.000000000000000000 ) ) ;
#11819 = ORIENTED_EDGE ( 'NONE', *, *, #10093, .F. ) ;
#11820 = CARTESIAN_POINT ( 'NONE',  ( 3.068288344391240763, -2.655262421758693314, 0.000000000000000000 ) ) ;
#11821 = ORIENTED_EDGE ( 'NONE', *, *, #12762, .T. ) ;
#11822 = CARTESIAN_POINT ( 'NONE',  ( 35.00000000000000000, 90.00000000000000000, -3.799999999999999378 ) ) ;
#11823 = CIRCLE ( 'NONE', #7012, 6.499999999999999112 ) ;
#11824 = AXIS2_PLACEMENT_3D ( 'NONE', #9536, #559, #4501 ) ;
#11825 = DIRECTION ( 'NONE',  ( -0.000000000000000000, -0.000000000000000000, -1.000000000000000000 ) ) ;
#11826 = LINE ( 'NONE', #12874, #8842 ) ;
#11827 = DIRECTION ( 'NONE',  ( 1.049727191973305517E-16, 0.5150380737757253025, -0.8571673013836857979 ) ) ;
#11828 = PLANE ( 'NONE',  #9408 ) ;
#11829 = ORIENTED_EDGE ( 'NONE', *, *, #7188, .F. ) ;
#11830 = PLANE ( 'NONE',  #12443 ) ;
#11831 = CARTESIAN_POINT ( 'NONE',  ( -28.99038105676692112, 50.21281292110204930, -1.000000000000000000 ) ) ;
#11832 = ORIENTED_EDGE ( 'NONE', *, *, #1331, .T. ) ;
#11833 = VERTEX_POINT ( 'NONE', #7975 ) ;
#11834 = CIRCLE ( 'NONE', #6186, 3.500000000000003109 ) ;
#11835 =( LENGTH_UNIT ( ) NAMED_UNIT ( * ) SI_UNIT ( .MILLI., .METRE. ) );
#11836 = ORIENTED_EDGE ( 'NONE', *, *, #3026, .T. ) ;
#11837 = EDGE_CURVE ( 'NONE', #1516, #8117, #11958, .T. ) ;
#11838 = EDGE_CURVE ( 'NONE', #6325, #10905, #12025, .T. ) ;
#11839 = CARTESIAN_POINT ( 'NONE',  ( 62.73514746974691292, 98.48596457872595522, 4.000000000000000000 ) ) ;
#11840 = CARTESIAN_POINT ( 'NONE',  ( 7.500000000000000000, 27.00000000000000000, 0.000000000000000000 ) ) ;
#11841 = ORIENTED_EDGE ( 'NONE', *, *, #9951, .F. ) ;
#11842 = VECTOR ( 'NONE', #7762, 1000.000000000000114 ) ;
#11843 = DIRECTION ( 'NONE',  ( -1.000000000000000000, 0.000000000000000000, 0.000000000000000000 ) ) ;
#11844 = VERTEX_POINT ( 'NONE', #1956 ) ;
#11845 = FACE_BOUND ( 'NONE', #6583, .T. ) ;
#11846 = ORIENTED_EDGE ( 'NONE', *, *, #9910, .F. ) ;
#11847 = CARTESIAN_POINT ( 'NONE',  ( 19.27821517812500574, 117.2309300971526937, 4.278125000614516615 ) ) ;
#11848 = VERTEX_POINT ( 'NONE', #9010 ) ;
#11849 = CARTESIAN_POINT ( 'NONE',  ( 1.000000000000000000, -5.473461295629626022, 0.000000000000000000 ) ) ;
#11850 = CARTESIAN_POINT ( 'NONE',  ( 35.00000000000000000, 126.0266567974326222, 3.987500000000000266 ) ) ;
#11851 = CIRCLE ( 'NONE', #7251, 3.349999999999995204 ) ;
#11852 = CARTESIAN_POINT ( 'NONE',  ( 19.40000000000002700, 62.98000740192551206, 3.387500001229033941 ) ) ;
#11853 = CARTESIAN_POINT ( 'NONE',  ( 3.556430356250015024, 90.00000000000000000, 3.003125000614517148 ) ) ;
#11854 = DIRECTION ( 'NONE',  ( 0.000000000000000000, 0.000000000000000000, 1.000000000000000000 ) ) ;
#11855 = ADVANCED_FACE ( 'NONE', ( #9931 ), #6793, .F. ) ;
#11856 = ORIENTED_EDGE ( 'NONE', *, *, #3497, .T. ) ;
#11857 = CARTESIAN_POINT ( 'NONE',  ( 35.00000000000000000, 126.0266567974326222, 4.887500000000001066 ) ) ;
#11858 = FACE_OUTER_BOUND ( 'NONE', #3102, .T. ) ;
#11859 = CARTESIAN_POINT ( 'NONE',  ( 13.53859087060910404, 112.9805567844265539, 2.999999999999999112 ) ) ;
#11860 = VECTOR ( 'NONE', #9311, 1000.000000000000000 ) ;
#11861 = ORIENTED_EDGE ( 'NONE', *, *, #81, .T. ) ;
#11862 = DIRECTION ( 'NONE',  ( -1.000000000000000000, 0.000000000000000000, 0.000000000000000000 ) ) ;
#11863 = ORIENTED_EDGE ( 'NONE', *, *, #12466, .F. ) ;
#11864 = FACE_OUTER_BOUND ( 'NONE', #9034, .T. ) ;
#11865 = CARTESIAN_POINT ( 'NONE',  ( 66.44356964374999563, 71.84604660189820891, 4.596875000614517148 ) ) ;
#11866 = ORIENTED_EDGE ( 'NONE', *, *, #59, .T. ) ;
#11867 = CARTESIAN_POINT ( 'NONE',  ( 66.44356964374998142, 108.1539533981018053, 4.671875000614516438 ) ) ;
#11868 = ADVANCED_FACE ( 'NONE', ( #5816 ), #5024, .T. ) ;
#11869 = LINE ( 'NONE', #1000, #4759 ) ;
#11870 = CIRCLE ( 'NONE', #3941, 3.500000000000003109 ) ;
#11871 = AXIS2_PLACEMENT_3D ( 'NONE', #2562, #4329, #7464 ) ;
#11872 = ADVANCED_FACE ( 'NONE', ( #9744 ), #12814, .F. ) ;
#11873 = DIRECTION ( 'NONE',  ( 0.000000000000000000, 0.000000000000000000, -1.000000000000000000 ) ) ;
#11874 = CARTESIAN_POINT ( 'NONE',  ( 1.040000000000000036, 0.000000000000000000, 0.000000000000000000 ) ) ;
#11875 = MANIFOLD_SOLID_BREP ( 'AdvancedHole1', #8654 ) ;
#11876 = DIRECTION ( 'NONE',  ( 0.000000000000000000, 0.000000000000000000, 1.000000000000000000 ) ) ;
#11877 = VECTOR ( 'NONE', #7577, 1000.000000000000000 ) ;
#11878 = DIRECTION ( 'NONE',  ( -0.000000000000000000, -0.000000000000000000, -1.000000000000000000 ) ) ;
#11879 = PLANE ( 'NONE',  #4739 ) ;
#11880 = VERTEX_POINT ( 'NONE', #6924 ) ;
#11881 = CARTESIAN_POINT ( 'NONE',  ( 35.00000000000000000, 90.00000000000000000, -5.000000000000000000 ) ) ;
#11882 = EDGE_LOOP ( 'NONE', ( #2948, #959, #2526, #4766 ) ) ;
#11883 = ADVANCED_FACE ( 'NONE', ( #10908 ), #836, .F. ) ;
#11884 = CARTESIAN_POINT ( 'NONE',  ( -65.16099272381319452, 29.63910161513775066, 0.000000000000000000 ) ) ;
#11885 = VECTOR ( 'NONE', #8273, 1000.000000000000000 ) ;
#11886 = CARTESIAN_POINT ( 'NONE',  ( 0.1038759689922479496, -3.348389132562988646, -0.8000000000000000444 ) ) ;
#11887 = CARTESIAN_POINT ( 'NONE',  ( 32.09707732552327286, 88.32801317409231956, -3.800000000000000266 ) ) ;
#11888 = CARTESIAN_POINT ( 'NONE',  ( 0.000000000000000000, 1.154700538379252350, -1.084202172485497162E-16 ) ) ;
#11889 = DIRECTION ( 'NONE',  ( 1.000000000000000000, 0.000000000000000000, 0.000000000000000000 ) ) ;
#11890 = VERTEX_POINT ( 'NONE', #11477 ) ;
#11891 = CARTESIAN_POINT ( 'NONE',  ( 35.00000000000000000, 90.00000000000000000, -8.000000000000000000 ) ) ;
#11892 = CYLINDRICAL_SURFACE ( 'NONE', #3356, 6.499999999999999112 ) ;
#11893 = ORIENTED_EDGE ( 'NONE', *, *, #2283, .T. ) ;
#11894 = VECTOR ( 'NONE', #7213, 1000.000000000000000 ) ;
#11895 = EDGE_LOOP ( 'NONE', ( #1406, #11389, #878, #576 ) ) ;
#11896 = VECTOR ( 'NONE', #10213, 1000.000000000000000 ) ;
#11897 = ORIENTED_EDGE ( 'NONE', *, *, #12124, .T. ) ;
#11898 = EDGE_CURVE ( 'NONE', #11106, #585, #6438, .T. ) ;
#11899 = LINE ( 'NONE', #7055, #3405 ) ;
#11900 = DIRECTION ( 'NONE',  ( -5.624500927088228034E-17, 1.370729058197317775E-18, 1.000000000000000000 ) ) ;
#11901 = VECTOR ( 'NONE', #6789, 1000.000000000000000 ) ;
#11902 = EDGE_LOOP ( 'NONE', ( #5824, #4929 ) ) ;
#11903 = CARTESIAN_POINT ( 'NONE',  ( 0.000000000000000000, 0.000000000000000000, 0.000000000000000000 ) ) ;
#11904 = ORIENTED_EDGE ( 'NONE', *, *, #2299, .T. ) ;
#11905 = EDGE_CURVE ( 'NONE', #9298, #12318, #12534, .T. ) ;
#11906 = CARTESIAN_POINT ( 'NONE',  ( 1.269999999999999796, 0.000000000000000000, 0.000000000000000000 ) ) ;
#11907 = ADVANCED_FACE ( 'NONE', ( #8104 ), #476, .T. ) ;
#11908 = EDGE_LOOP ( 'NONE', ( #11524, #5167, #1337, #896 ) ) ;
#11909 = CARTESIAN_POINT ( 'NONE',  ( 3.556430356250015024, 90.00000000000000000, 3.003125000614517148 ) ) ;
#11910 = PRODUCT_DEFINITION_SHAPE ( 'NONE', 'NONE',  #12960 ) ;
#11911 = ORIENTED_EDGE ( 'NONE', *, *, #841, .T. ) ;
#11912 = AXIS2_PLACEMENT_3D ( 'NONE', #10640, #4694, #7821 ) ;
#11913 = DIRECTION ( 'NONE',  ( 1.000000000000000000, -6.405132834375904028E-15, 0.000000000000000000 ) ) ;
#11914 = DIRECTION ( 'NONE',  ( -1.000000000000000000, -0.000000000000000000, -0.000000000000000000 ) ) ;
#11915 = CARTESIAN_POINT ( 'NONE',  ( 45.00000000000000000, -5.901290925839664858, -5.750000000000000000 ) ) ;
#11916 = CARTESIAN_POINT ( 'NONE',  ( 19.40000000000000924, 117.0199925980744666, 4.137500001229033941 ) ) ;
#11917 = ADVANCED_FACE ( 'NONE', ( #3576 ), #4182, .T. ) ;
#11918 = FACE_OUTER_BOUND ( 'NONE', #10791, .T. ) ;
#11919 = ORIENTED_EDGE ( 'NONE', *, *, #5954, .F. ) ;
#11920 = AXIS2_PLACEMENT_3D ( 'NONE', #12594, #2585, #11732 ) ;
#11921 = DIRECTION ( 'NONE',  ( 0.000000000000000000, 0.000000000000000000, 1.000000000000000000 ) ) ;
#11922 = DIRECTION ( 'NONE',  ( -1.000000000000000000, -0.000000000000000000, -0.000000000000000000 ) ) ;
#11923 = CARTESIAN_POINT ( 'NONE',  ( 17.58542467432373257, 116.1886173078550542, 3.000000000000001332 ) ) ;
#11924 = ORIENTED_EDGE ( 'NONE', *, *, #7084, .T. ) ;
#11925 =( BOUNDED_CURVE ( )  B_SPLINE_CURVE ( 2, ( #1645, #8391, #11520, #6610, #12442, #10609, #6413 ),
 .UNSPECIFIED., .F., .F. ) 
 B_SPLINE_CURVE_WITH_KNOTS ( ( 3, 2, 2, 3 ),
 ( 0.1000000000000001860, 0.1333333333333334425, 0.1666666666666666852, 0.2000000000000000111 ),
 .UNSPECIFIED. ) 
 CURVE ( )  GEOMETRIC_REPRESENTATION_ITEM ( )  RATIONAL_B_SPLINE_CURVE ( ( 0.9999999999999992228, 0.8660254037844394848, 1.000000000000000000, 0.8660254037844387076, 1.000000000000000000, 0.8660254037844388186, 0.9999999999999998890 ) ) 
 REPRESENTATION_ITEM ( '' )  );
#11926 = CARTESIAN_POINT ( 'NONE',  ( 1.040000000000000036, -0.5773502691896256200, -1.000000000000000000 ) ) ;
#11927 = ORIENTED_EDGE ( 'NONE', *, *, #8286, .T. ) ;
#11928 = DIRECTION ( 'NONE',  ( -0.000000000000000000, 1.000000000000000000, -0.000000000000000000 ) ) ;
#11929 = CARTESIAN_POINT ( 'NONE',  ( 50.72178482187499071, 117.2309300971526937, 4.709375000614516971 ) ) ;
#11930 = EDGE_CURVE ( 'NONE', #6209, #5251, #4485, .T. ) ;
#11931 = ORIENTED_EDGE ( 'NONE', *, *, #3298, .T. ) ;
#11932 = CARTESIAN_POINT ( 'NONE',  ( 35.00000000000000711, 53.69209320379640360, 3.171875000614517326 ) ) ;
#11933 = CARTESIAN_POINT ( 'NONE',  ( -2.387319993259524598, -4.036502139894371233, 0.000000000000000000 ) ) ;
#11934 = LINE ( 'NONE', #8925, #8663 ) ;
#11935 = CARTESIAN_POINT ( 'NONE',  ( 7.264852530253062213, 98.48596457872582732, 2.333333333333333037 ) ) ;
#11936 = DIRECTION ( 'NONE',  ( -1.000000000000000000, 0.000000000000000000, 0.000000000000000000 ) ) ;
#11937 = PLANE ( 'NONE',  #8163 ) ;
#11938 = DIRECTION ( 'NONE',  ( -1.000000000000000000, 0.000000000000000000, -0.000000000000000000 ) ) ;
#11939 = ADVANCED_FACE ( 'NONE', ( #10498 ), #7556, .T. ) ;
#11940 = VERTEX_POINT ( 'NONE', #11168 ) ;
#11941 = CARTESIAN_POINT ( 'NONE',  ( 3.033375984251970081, -8.673617379884035472E-16, 0.000000000000000000 ) ) ;
#11942 = VERTEX_POINT ( 'NONE', #409 ) ;
#11943 = CARTESIAN_POINT ( 'NONE',  ( 34.25000000000000000, 93.41869858279433458, 6.000000000000000000 ) ) ;
#11944 = AXIS2_PLACEMENT_3D ( 'NONE', #3074, #1829, #7778 ) ;
#11945 = PLANE ( 'NONE',  #9986 ) ;
#11946 = LINE ( 'NONE', #6975, #3635 ) ;
#11947 = LINE ( 'NONE', #1944, #3009 ) ;
#11948 = ORIENTED_EDGE ( 'NONE', *, *, #4918, .F. ) ;
#11949 = CARTESIAN_POINT ( 'NONE',  ( 1.625004804578465745, -6.241943558307532669, -0.8000000000000000444 ) ) ;
#11950 = DIRECTION ( 'NONE',  ( 0.000000000000000000, 0.000000000000000000, 1.000000000000000000 ) ) ;
#11951 = EDGE_CURVE ( 'NONE', #1608, #5251, #5219, .T. ) ;
#11952 = VERTEX_POINT ( 'NONE', #3512 ) ;
#11953 = AXIS2_PLACEMENT_3D ( 'NONE', #1977, #4009, #11976 ) ;
#11954 =( NAMED_UNIT ( * ) PLANE_ANGLE_UNIT ( ) SI_UNIT ( $, .RADIAN. ) );
#11955 =( LENGTH_UNIT ( ) NAMED_UNIT ( * ) SI_UNIT ( .MILLI., .METRE. ) );
#11956 = EDGE_CURVE ( 'NONE', #12821, #3363, #6503, .T. ) ;
#11957 = EDGE_LOOP ( 'NONE', ( #10373, #5537, #12664, #6412 ) ) ;
#11958 = LINE ( 'NONE', #3800, #9437 ) ;
#11959 = ORIENTED_EDGE ( 'NONE', *, *, #57, .F. ) ;
#11960 = PLANE ( 'NONE',  #9668 ) ;
#11961 = CARTESIAN_POINT ( 'NONE',  ( 35.00000000000000000, 90.00000000000000000, -3.000000000000000000 ) ) ;
#11962 = EDGE_LOOP ( 'NONE', ( #3829, #1509 ) ) ;
#11963 = AXIS2_PLACEMENT_3D ( 'NONE', #7184, #4185, #3277 ) ;
#11964 = ORIENTED_EDGE ( 'NONE', *, *, #3108, .T. ) ;
#11965 = B_SPLINE_CURVE_WITH_KNOTS ( 'NONE', 3,
 ( #3825, #3034, #4738, #10750 ),
 .UNSPECIFIED., .F., .F.,
 ( 4, 4 ),
 ( 0.000000000000000000, 1.000000000000000000 ),
 .UNSPECIFIED. ) ;
#11966 = CARTESIAN_POINT ( 'NONE',  ( 9.136132550659251450, 74.79933025939541835, -0.9999999999999970024 ) ) ;
#11967 = VERTEX_POINT ( 'NONE', #1533 ) ;
#11968 = CARTESIAN_POINT ( 'NONE',  ( 1.599999999999999867, -4.873461295629625489, -0.8000000000000000444 ) ) ;
#11969 = EDGE_CURVE ( 'NONE', #992, #1427, #1500, .T. ) ;
#11970 = ORIENTED_EDGE ( 'NONE', *, *, #11602, .F. ) ;
#11971 = CARTESIAN_POINT ( 'NONE',  ( 20.00000000000000355, 2.000000000000000000, 10.00000000000000000 ) ) ;
#11972 = ORIENTED_EDGE ( 'NONE', *, *, #7806, .T. ) ;
#11973 = MECHANICAL_DESIGN_GEOMETRIC_PRESENTATION_REPRESENTATION (  '', ( #1945 ), #12609 ) ;
#11974 = DIRECTION ( 'NONE',  ( 0.000000000000000000, 0.000000000000000000, 1.000000000000000000 ) ) ;
#11975 = CARTESIAN_POINT ( 'NONE',  ( 3.556430356250015024, 90.00000000000000000, 3.903125000614517504 ) ) ;
#11976 = DIRECTION ( 'NONE',  ( -1.000000000000000000, 0.000000000000000000, 0.000000000000000000 ) ) ;
#11977 = CARTESIAN_POINT ( 'NONE',  ( 35.00000000000000000, 126.0266567974326222, 3.650000001229034119 ) ) ;
#11978 = VECTOR ( 'NONE', #3917, 1000.000000000000000 ) ;
#11979 = ADVANCED_FACE ( 'NONE', ( #8412 ), #2224, .T. ) ;
#11980 = CARTESIAN_POINT ( 'NONE',  ( 64.54728993811707483, 100.7543353701752125, 2.858851390224067313 ) ) ;
#11981 = ORIENTED_EDGE ( 'NONE', *, *, #1995, .T. ) ;
#11982 = CARTESIAN_POINT ( 'NONE',  ( 5.000000000000004441, 30.00000000000000000, 2.500000000000000444 ) ) ;
#11983 = CARTESIAN_POINT ( 'NONE',  ( 35.00000000000000000, 90.00000000000000000, 4.000000000000000000 ) ) ;
#11984 = CARTESIAN_POINT ( 'NONE',  ( 48.20636397115843153, 118.4025818652226860, 3.000000000000001776 ) ) ;
#11985 = VERTEX_POINT ( 'NONE', #2089 ) ;
#11986 = VECTOR ( 'NONE', #11827, 999.9999999999998863 ) ;
#11987 = CARTESIAN_POINT ( 'NONE',  ( 3.800000000000015365, 90.00000000000000000, 5.000000000000000000 ) ) ;
#11988 = ORIENTED_EDGE ( 'NONE', *, *, #10440, .T. ) ;
#11989 = CARTESIAN_POINT ( 'NONE',  ( 3.556430356250015024, 90.00000000000000000, 4.831250000614517148 ) ) ;
#11990 = CARTESIAN_POINT ( 'NONE',  ( 50.72178482187499071, 117.2309300971526937, 3.753125000614517592 ) ) ;
#11991 = ORIENTED_EDGE ( 'NONE', *, *, #6960, .T. ) ;
#11993 = CARTESIAN_POINT ( 'NONE',  ( 35.00000000000000711, 53.69209320379640360, 4.521875000614516971 ) ) ;
#11992 = PRODUCT_DEFINITION_FORMATION_WITH_SPECIFIED_SOURCE ( 'ANY', '', #5413, .NOT_KNOWN. ) ;
#11994 = LINE ( 'NONE', #8983, #5996 ) ;
#11995 = EDGE_CURVE ( 'NONE', #8496, #4743, #442, .T. ) ;
#11996 = DIRECTION ( 'NONE',  ( 0.000000000000000000, 0.000000000000000000, 1.000000000000000000 ) ) ;
#11997 = EDGE_CURVE ( 'NONE', #10802, #2240, #544, .T. ) ;
#11998 = CIRCLE ( 'NONE', #12420, 1.000000000000000000 ) ;
#11999 = AXIS2_PLACEMENT_3D ( 'NONE', #2790, #12921, #6962 ) ;
#12000 = CARTESIAN_POINT ( 'NONE',  ( 64.54728994471078352, 100.7543353520590870, 2.802601390178781404 ) ) ;
#12001 = CARTESIAN_POINT ( 'NONE',  ( 35.00000000000000000, 90.00000000000000000, -0.9999999999999970024 ) ) ;
#12002 = MANIFOLD_SOLID_BREP ( 'Hex', #3437 ) ;
#12003 = DIRECTION ( 'NONE',  ( -1.000000000000000000, 0.000000000000000000, 0.000000000000000000 ) ) ;
#12004 = CARTESIAN_POINT ( 'NONE',  ( 48.49999999999995737, 90.00000000000000000, -10.00000000000000000 ) ) ;
#12005 = AXIS2_PLACEMENT_3D ( 'NONE', #10653, #572, #4579 ) ;
#12006 = PLANE ( 'NONE',  #10168 ) ;
#12007 = ORIENTED_EDGE ( 'NONE', *, *, #9072, .T. ) ;
#12008 = VECTOR ( 'NONE', #5432, 1000.000000000000114 ) ;
#12009 = CARTESIAN_POINT ( 'NONE',  ( 62.42406877266672183, 99.43633196372844907, 4.000000000000000000 ) ) ;
#12010 = ORIENTED_EDGE ( 'NONE', *, *, #2964, .T. ) ;
#12011 = FACE_OUTER_BOUND ( 'NONE', #11805, .T. ) ;
#12012 = CARTESIAN_POINT ( 'NONE',  ( 31.50000000000000711, 90.00000000000000000, 22.38477631085024555 ) ) ;
#12013 = PLANE ( 'NONE',  #9102 ) ;
#12014 = CIRCLE ( 'NONE', #1571, 1.500000000000001332 ) ;
#12015 = PRODUCT_DEFINITION_SHAPE ( 'NONE', 'NONE',  #12973 ) ;
#12016 = EDGE_CURVE ( 'NONE', #11426, #3209, #6200, .T. ) ;
#12017 = CARTESIAN_POINT ( 'NONE',  ( 1.040000000000000036, 1.154700538379252350, -1.084202172485497162E-16 ) ) ;
#12018 = AXIS2_PLACEMENT_3D ( 'NONE', #1098, #11243, #12035 ) ;
#12019 = EDGE_LOOP ( 'NONE', ( #7020, #9556, #578, #5698 ) ) ;
#12020 = DIRECTION ( 'NONE',  ( -0.000000000000000000, -0.000000000000000000, -1.000000000000000000 ) ) ;
#12021 = DIRECTION ( 'NONE',  ( 1.000000000000000000, -4.270088556250602685E-15, 0.000000000000000000 ) ) ;
#12022 = ORIENTED_EDGE ( 'NONE', *, *, #10959, .T. ) ;
#12023 = CARTESIAN_POINT ( 'NONE',  ( 50.00000000000000000, 2.000000000000000000, -10.00000000000000000 ) ) ;
#12024 = ORIENTED_EDGE ( 'NONE', *, *, #8706, .F. ) ;
#12025 = LINE ( 'NONE', #3864, #862 ) ;
#12027 = ORIENTED_EDGE ( 'NONE', *, *, #5911, .T. ) ;
#12026 = CIRCLE ( 'NONE', #3263, 1.500000000000001332 ) ;
#12028 = CARTESIAN_POINT ( 'NONE',  ( 35.00000000000000711, 53.97334320256736362, 4.212500000000000355 ) ) ;
#12029 = DIRECTION ( 'NONE',  ( -1.000000000000000000, -0.000000000000000000, -0.000000000000000000 ) ) ;
#12030 = ADVANCED_FACE ( 'NONE', ( #7811 ), #8107, .T. ) ;
#12031 = ORIENTED_EDGE ( 'NONE', *, *, #12704, .F. ) ;
#12032 = EDGE_CURVE ( 'NONE', #2817, #6997, #7266, .T. ) ;
#12033 = ADVANCED_FACE ( 'NONE', ( #9505 ), #4219, .F. ) ;
#12034 = ORIENTED_EDGE ( 'NONE', *, *, #10700, .F. ) ;
#12035 = DIRECTION ( 'NONE',  ( 0.000000000000000000, 0.000000000000000000, 1.000000000000000000 ) ) ;
#12036 = ORIENTED_EDGE ( 'NONE', *, *, #10071, .F. ) ;
#12037 = SHAPE_DEFINITION_REPRESENTATION ( #11264, #4597 ) ;
#12038 = CARTESIAN_POINT ( 'NONE',  ( 19.27821517812500574, 117.2309300971526937, 3.828125000614516882 ) ) ;
#12039 = VERTEX_POINT ( 'NONE', #3370 ) ;
#12040 = CARTESIAN_POINT ( 'NONE',  ( 25.00000000000000355, 0.000000000000000000, 4.249999999999998224 ) ) ;
#12041 = EDGE_LOOP ( 'NONE', ( #299, #8993, #11459, #1797 ) ) ;
#12042 = DIRECTION ( 'NONE',  ( -0.000000000000000000, 1.000000000000000000, -0.000000000000000000 ) ) ;
#12043 = CARTESIAN_POINT ( 'NONE',  ( 66.44356964374999563, 90.00000000000000000, 4.128125000614517148 ) ) ;
#12044 = LINE ( 'NONE', #7185, #6941 ) ;
#12045 = CARTESIAN_POINT ( 'NONE',  ( 1.750000000000000000, 0.000000000000000000, 0.000000000000000000 ) ) ;
#12046 = DIRECTION ( 'NONE',  ( 0.000000000000000000, 0.000000000000000000, 1.000000000000000000 ) ) ;
#12047 = EDGE_CURVE ( 'NONE', #3601, #3649, #6296, .T. ) ;
#12048 = CIRCLE ( 'NONE', #7031, 1.499999999999999556 ) ;
#12049 = FACE_OUTER_BOUND ( 'NONE', #8564, .T. ) ;
#12050 = ORIENTED_EDGE ( 'NONE', *, *, #12730, .F. ) ;
#12051 = CARTESIAN_POINT ( 'NONE',  ( 50.72178482187499071, 117.2309300971526937, 4.709375000614516971 ) ) ;
#12052 = LINE ( 'NONE', #3099, #1877 ) ;
#12053 = DIRECTION ( 'NONE',  ( -0.000000000000000000, -0.000000000000000000, -1.000000000000000000 ) ) ;
#12054 = ORIENTED_EDGE ( 'NONE', *, *, #12016, .F. ) ;
#12055 = CARTESIAN_POINT ( 'NONE',  ( 66.19999999999993179, 71.98667160128364628, 3.837499999999999911 ) ) ;
#12056 = ORIENTED_EDGE ( 'NONE', *, *, #6114, .F. ) ;
#12057 = AXIS2_PLACEMENT_3D ( 'NONE', #6810, #4855, #1782 ) ;
#12058 = DIRECTION ( 'NONE',  ( 1.000000000000000000, -0.000000000000000000, -0.000000000000000000 ) ) ;
#12059 = UNCERTAINTY_MEASURE_WITH_UNIT (LENGTH_MEASURE( 1.000000000000000082E-05 ), #6222, 'distance_accuracy_value', 'NONE');
#12060 = CARTESIAN_POINT ( 'NONE',  ( 3.556430356250015024, 90.00000000000000000, 3.003125000614517148 ) ) ;
#12061 = ORIENTED_EDGE ( 'NONE', *, *, #2653, .F. ) ;
#12062 = CARTESIAN_POINT ( 'NONE',  ( 3.556430356250015024, 90.00000000000000000, 3.959375000614517415 ) ) ;
#12063 = CARTESIAN_POINT ( 'NONE',  ( 25.00000000000000355, -5.000000000000000000, -5.750000000000000000 ) ) ;
#12064 = EDGE_CURVE ( 'NONE', #8179, #10269, #9310, .T. ) ;
#12065 = PLANE ( 'NONE',  #8553 ) ;
#12066 = VECTOR ( 'NONE', #6298, 1000.000000000000000 ) ;
#12067 =( LENGTH_UNIT ( ) NAMED_UNIT ( * ) SI_UNIT ( .MILLI., .METRE. ) );
#12068 = DIRECTION ( 'NONE',  ( 0.000000000000000000, 0.000000000000000000, 1.000000000000000000 ) ) ;
#12069 = DIRECTION ( 'NONE',  ( 0.9995191440486532741, -0.03100775193798452692, 0.000000000000000000 ) ) ;
#12070 = EDGE_CURVE ( 'NONE', #11441, #7451, #7572, .T. ) ;
#12071 = EDGE_CURVE ( 'NONE', #946, #2543, #11597, .T. ) ;
#12072 = CARTESIAN_POINT ( 'NONE',  ( 35.00000000000000000, 90.00000000000000000, 6.000000000000000000 ) ) ;
#12073 = LINE ( 'NONE', #5200, #4528 ) ;
#12074 = ORIENTED_EDGE ( 'NONE', *, *, #8856, .F. ) ;
#12075 = SPHERICAL_SURFACE ( 'NONE', #12691, 3.351416843938785028 ) ;
#12076 = ORIENTED_EDGE ( 'NONE', *, *, #12308, .T. ) ;
#12077 = EDGE_CURVE ( 'NONE', #8914, #2081, #2773, .T. ) ;
#12078 = DIRECTION ( 'NONE',  ( 1.000000000000000000, 0.000000000000000000, 0.000000000000000000 ) ) ;
#12079 = DIRECTION ( 'NONE',  ( 1.000000000000000000, 0.000000000000000000, -0.000000000000000000 ) ) ;
#12080 = CARTESIAN_POINT ( 'NONE',  ( -60.38397459621558738, 30.66506350946110260, 0.000000000000000000 ) ) ;
#12081 = VECTOR ( 'NONE', #10519, 1000.000000000000000 ) ;
#12082 = UNCERTAINTY_MEASURE_WITH_UNIT (LENGTH_MEASURE( 1.000000000000000082E-05 ), #7526, 'distance_accuracy_value', 'NONE');
#12083 = VERTEX_POINT ( 'NONE', #9571 ) ;
#12084 = DIRECTION ( 'NONE',  ( -1.000000000000000000, 0.000000000000000000, 0.000000000000000000 ) ) ;
#12085 = DIRECTION ( 'NONE',  ( 0.8660254037844362651, 0.5000000000000042188, 0.000000000000000000 ) ) ;
#12086 = ORIENTED_EDGE ( 'NONE', *, *, #5564, .F. ) ;
#12087 =( NAMED_UNIT ( * ) SI_UNIT ( $, .STERADIAN. ) SOLID_ANGLE_UNIT ( ) );
#12088 = CARTESIAN_POINT ( 'NONE',  ( 36.50000000000001421, 79.80000000000001137, 8.000000000000000000 ) ) ;
#12089 = ORIENTED_EDGE ( 'NONE', *, *, #109, .F. ) ;
#12090 = DIRECTION ( 'NONE',  ( 0.000000000000000000, 0.000000000000000000, 1.000000000000000000 ) ) ;
#12091 = ORIENTED_EDGE ( 'NONE', *, *, #9064, .T. ) ;
#12092 = ADVANCED_FACE ( 'NONE', ( #7735 ), #7542, .T. ) ;
#12093 = DIRECTION ( 'NONE',  ( -0.5000000000000043299, 0.8660254037844362651, 0.000000000000000000 ) ) ;
#12094 = ORIENTED_EDGE ( 'NONE', *, *, #109, .T. ) ;
#12095 = ORIENTED_EDGE ( 'NONE', *, *, #3152, .T. ) ;
#12097 = DIRECTION ( 'NONE',  ( -1.000000000000000000, 0.000000000000000000, 0.000000000000000000 ) ) ;
#12096 = VECTOR ( 'NONE', #7420, 1000.000000000000000 ) ;
#12098 = ORIENTED_EDGE ( 'NONE', *, *, #4074, .F. ) ;
#12099 = CARTESIAN_POINT ( 'NONE',  ( 19.27821517812503060, 62.76906990284727783, 4.428125000614516971 ) ) ;
#12100 = VECTOR ( 'NONE', #1394, 1000.000000000000000 ) ;
#12101 = ORIENTED_EDGE ( 'NONE', *, *, #9318, .T. ) ;
#12102 = EDGE_CURVE ( 'NONE', #10802, #4183, #5644, .T. ) ;
#12103 = CARTESIAN_POINT ( 'NONE',  ( 50.60000000000001563, 62.98000740192552627, 3.462500001229034563 ) ) ;
#12104 = FACE_OUTER_BOUND ( 'NONE', #6866, .T. ) ;
#12105 = ORIENTED_EDGE ( 'NONE', *, *, #6088, .F. ) ;
#12106 = CYLINDRICAL_SURFACE ( 'NONE', #11519, 31.19999999999999929 ) ;
#12107 = CARTESIAN_POINT ( 'NONE',  ( 3.556430356250015024, 90.00000000000000000, 4.803125000614516971 ) ) ;
#12108 = EDGE_CURVE ( 'NONE', #2190, #10351, #4235, .T. ) ;
#12109 = CARTESIAN_POINT ( 'NONE',  ( 9.650000000000000355, 0.000000000000000000, 1.219500000000000028 ) ) ;
#12110 = VECTOR ( 'NONE', #10534, 1000.000000000000114 ) ;
#12111 = CARTESIAN_POINT ( 'NONE',  ( 3.800000000000015365, 90.00000000000000000, 3.312500001229034652 ) ) ;
#12112 = B_SPLINE_CURVE_WITH_KNOTS ( 'NONE', 3,
 ( #4737, #1726, #2716, #3892 ),
 .UNSPECIFIED., .F., .F.,
 ( 4, 4 ),
 ( 0.000000000000000000, 1.000000000000000000 ),
 .UNSPECIFIED. ) ;
#12113 = MANIFOLD_SOLID_BREP ( 'AdvancedHole2', #9907 ) ;
#12114 =( REPRESENTATION_RELATIONSHIP ('NONE','NONE', #1997, #7342 ) REPRESENTATION_RELATIONSHIP_WITH_TRANSFORMATION ( #11373 )SHAPE_REPRESENTATION_RELATIONSHIP( ) );
#12115 = CARTESIAN_POINT ( 'NONE',  ( 35.00000000000000000, 90.00000000000000000, -3.799999999999999822 ) ) ;
#12116 = EDGE_LOOP ( 'NONE', ( #6447, #10506 ) ) ;
#12117 = CARTESIAN_POINT ( 'NONE',  ( 19.40000000000000924, 117.0199925980744666, 4.025000000000000355 ) ) ;
#12118 = DIRECTION ( 'NONE',  ( 1.000000000000000000, 0.000000000000000000, 5.337610695313252124E-17 ) ) ;
#12119 = CARTESIAN_POINT ( 'NONE',  ( 0.000000000000000000, 0.000000000000000000, -0.8000000000000000444 ) ) ;
#12120 = VERTEX_POINT ( 'NONE', #3752 ) ;
#12121 = VECTOR ( 'NONE', #1085, 1000.000000000000000 ) ;
#12122 = FACE_OUTER_BOUND ( 'NONE', #4721, .T. ) ;
#12123 = EDGE_LOOP ( 'NONE', ( #2167, #2658, #3229, #10061 ) ) ;
#12124 = EDGE_CURVE ( 'NONE', #11182, #9021, #9864, .T. ) ;
#12125 = DIRECTION ( 'NONE',  ( 1.000000000000000000, 0.000000000000000000, -0.000000000000000000 ) ) ;
#12126 = DIRECTION ( 'NONE',  ( -0.000000000000000000, -0.000000000000000000, -1.000000000000000000 ) ) ;
#12128 = VERTEX_POINT ( 'NONE', #11659 ) ;
#12127 = ADVANCED_FACE ( 'NONE', ( #7672 ), #6619, .F. ) ;
#12129 = CARTESIAN_POINT ( 'NONE',  ( 3.556430356250028790, 71.84604660189818048, 3.096875000614517592 ) ) ;
#12130 = DIRECTION ( 'NONE',  ( -1.000000000000000000, 0.000000000000000000, 0.000000000000000000 ) ) ;
#12131 = PRODUCT_DEFINITION_SHAPE ( 'NONE', 'NONE',  #12967 ) ;
#12132 = CARTESIAN_POINT ( 'NONE',  ( 45.00000000000000000, 2.000000000000001332, -4.150000000000009237 ) ) ;
#12133 = VECTOR ( 'NONE', #7759, 1000.000000000000000 ) ;
#12134 = CARTESIAN_POINT ( 'NONE',  ( 8.499999999999998224, 79.07477288111861924, -1.000000000000000222 ) ) ;
#12135 = CARTESIAN_POINT ( 'NONE',  ( 44.16515138991168499, 86.00000000000000000, -18.00000000000000355 ) ) ;
#12136 = LINE ( 'NONE', #8084, #7844 ) ;
#12137 = ADVANCED_FACE ( 'NONE', ( #660 ), #4791, .T. ) ;
#12138 = CONICAL_SURFACE ( 'NONE', #7954, 1.219500000000000028, 0.7853981633974487231 ) ;
#12139 = PLANE ( 'NONE',  #4198 ) ;
#12140 = CARTESIAN_POINT ( 'NONE',  ( 7.369500000000001272, 0.000000000000000000, 1.499999999999999778 ) ) ;
#12141 = EDGE_LOOP ( 'NONE', ( #9561, #5369, #2592, #10461 ) ) ;
#12142 = PLANE ( 'NONE',  #3304 ) ;
#12143 = ORIENTED_EDGE ( 'NONE', *, *, #4483, .F. ) ;
#12144 = EDGE_CURVE ( 'NONE', #7589, #11688, #238, .T. ) ;
#12145 = VECTOR ( 'NONE', #7989, 1000.000000000000000 ) ;
#12146 = FACE_OUTER_BOUND ( 'NONE', #2412, .T. ) ;
#12147 = DIRECTION ( 'NONE',  ( -0.000000000000000000, 1.000000000000000000, -0.000000000000000000 ) ) ;
#12148 = CARTESIAN_POINT ( 'NONE',  ( 35.00000000000000000, 90.00000000000000000, 1.000000000000000000 ) ) ;
#12149 = ORIENTED_EDGE ( 'NONE', *, *, #913, .T. ) ;
#12150 = CARTESIAN_POINT ( 'NONE',  ( 5.000000000000004441, 30.00000000000000000, -2.500000000000000444 ) ) ;
#12151 = CARTESIAN_POINT ( 'NONE',  ( 19.40000000000000924, 117.0199925980744666, 4.137500001229033941 ) ) ;
#12152 = VERTEX_POINT ( 'NONE', #7795 ) ;
#12153 = EDGE_CURVE ( 'NONE', #2507, #1106, #9239, .T. ) ;
#12154 = FACE_OUTER_BOUND ( 'NONE', #3588, .T. ) ;
#12155 = ORIENTED_EDGE ( 'NONE', *, *, #1444, .T. ) ;
#12156 = MANIFOLD_SOLID_BREP ( 'Notch', #1111 ) ;
#12157=STYLED_ITEM('',(#13009),#12002);
#12158 = DIRECTION ( 'NONE',  ( -0.000000000000000000, 0.000000000000000000, 1.000000000000000000 ) ) ;
#12159 = ORIENTED_EDGE ( 'NONE', *, *, #310, .T. ) ;
#12160 = FACE_OUTER_BOUND ( 'NONE', #3359, .T. ) ;
#12161 = CARTESIAN_POINT ( 'NONE',  ( 31.50000000000000711, 90.00000000000000000, 4.000000000000000000 ) ) ;
#12162 = VERTEX_POINT ( 'NONE', #4072 ) ;
#12163 = EDGE_CURVE ( 'NONE', #10459, #3765, #2708, .T. ) ;
#12164 = ORIENTED_EDGE ( 'NONE', *, *, #3205, .F. ) ;
#12165 = AXIS2_PLACEMENT_3D ( 'NONE', #9422, #10343, #2367 ) ;
#12166 = DIRECTION ( 'NONE',  ( -0.000000000000000000, -1.000000000000000000, -0.000000000000000000 ) ) ;
#12167 = ORIENTED_EDGE ( 'NONE', *, *, #7200, .F. ) ;
#12168 = CARTESIAN_POINT ( 'NONE',  ( 66.20000000000000284, 71.98667160128370313, 4.400000001229034119 ) ) ;
#12169 = ORIENTED_EDGE ( 'NONE', *, *, #2930, .T. ) ;
#12170 = CYLINDRICAL_SURFACE ( 'NONE', #1953, 2.849999999999999645 ) ;
#12171 = CARTESIAN_POINT ( 'NONE',  ( 1.000000000000000000, -4.273461295629625845, -0.8000000000000000444 ) ) ;
#12172 = EDGE_LOOP ( 'NONE', ( #2597, #5433, #944, #11086 ) ) ;
#12173 = DIRECTION ( 'NONE',  ( 0.000000000000000000, 0.000000000000000000, 1.000000000000000000 ) ) ;
#12174 = CARTESIAN_POINT ( 'NONE',  ( 50.72178482187499071, 117.2309300971526937, 3.753125000614517592 ) ) ;
#12175 = CARTESIAN_POINT ( 'NONE',  ( 35.75000000000000711, 92.49999999999998579, 6.000000000000000000 ) ) ;
#12176 = AXIS2_PLACEMENT_3D ( 'NONE', #9681, #2693, #776 ) ;
#12177 = DIRECTION ( 'NONE',  ( 0.000000000000000000, 0.000000000000000000, 1.000000000000000000 ) ) ;
#12178 =( NAMED_UNIT ( * ) SI_UNIT ( $, .STERADIAN. ) SOLID_ANGLE_UNIT ( ) );
#12179 = CARTESIAN_POINT ( 'NONE',  ( 0.000000000000000000, 0.000000000000000000, -10.00000000000000000 ) ) ;
#12180 = VERTEX_POINT ( 'NONE', #4137 ) ;
#12181 = CARTESIAN_POINT ( 'NONE',  ( 19.27821517812500574, 117.2309300971526937, 4.784375000614516260 ) ) ;
#12182 = EDGE_CURVE ( 'NONE', #998, #4984, #10012, .T. ) ;
#12183 = CARTESIAN_POINT ( 'NONE',  ( 1.649999999999999911, 1.499999999999999112, 0.000000000000000000 ) ) ;
#12184 = ORIENTED_EDGE ( 'NONE', *, *, #12198, .T. ) ;
#12185 = DIRECTION ( 'NONE',  ( -1.000000000000000000, 0.000000000000000000, 0.000000000000000000 ) ) ;
#12186 = ORIENTED_EDGE ( 'NONE', *, *, #6067, .F. ) ;
#12187 = CARTESIAN_POINT ( 'NONE',  ( 7.500000000000000000, 30.00000000000000000, 1.499999999999999556 ) ) ;
#12188 = AXIS2_PLACEMENT_3D ( 'NONE', #5115, #10222, #2185 ) ;
#12189 = CARTESIAN_POINT ( 'NONE',  ( 19.27821517812503060, 62.76906990284727783, 3.978125000614516793 ) ) ;
#12190 = EDGE_LOOP ( 'NONE', ( #7400, #9017, #2180, #11970 ) ) ;
#12191 = DIRECTION ( 'NONE',  ( 1.000000000000000000, 0.000000000000000000, 0.000000000000000000 ) ) ;
#12192 = DIRECTION ( 'NONE',  ( -0.000000000000000000, 1.000000000000000000, -0.000000000000000000 ) ) ;
#12193 = DIRECTION ( 'NONE',  ( 0.000000000000000000, 0.000000000000000000, 1.000000000000000000 ) ) ;
#12194 = STYLED_ITEM ( 'NONE', ( #7970 ), #1374 ) ;
#12195 = EDGE_CURVE ( 'NONE', #655, #216, #21, .T. ) ;
#12196 = FACE_OUTER_BOUND ( 'NONE', #5152, .T. ) ;
#12197 = CIRCLE ( 'NONE', #10935, 1.499999999999999778 ) ;
#12198 = EDGE_CURVE ( 'NONE', #9021, #919, #9883, .T. ) ;
#12199 = DIRECTION ( 'NONE',  ( -1.000000000000000000, -0.000000000000000000, -0.000000000000000000 ) ) ;
#12200 = DIRECTION ( 'NONE',  ( 0.000000000000000000, 0.000000000000000000, -1.000000000000000000 ) ) ;
#12201 = CARTESIAN_POINT ( 'NONE',  ( -6.666666666666660745, -5.000000000000000000, 1.499999999999999556 ) ) ;
#12202 = AXIS2_PLACEMENT_3D ( 'NONE', #7128, #11308, #7062 ) ;
#12203 = DIRECTION ( 'NONE',  ( -0.000000000000000000, 1.000000000000000000, -0.000000000000000000 ) ) ;
#12204 = DIRECTION ( 'NONE',  ( 0.000000000000000000, 0.000000000000000000, 1.000000000000000000 ) ) ;
#12205 = VERTEX_POINT ( 'NONE', #7136 ) ;
#12206 = DIRECTION ( 'NONE',  ( -0.5000000000000043299, 0.8660254037844362651, 0.000000000000000000 ) ) ;
#12207 = VERTEX_POINT ( 'NONE', #2900 ) ;
#12208 = CIRCLE ( 'NONE', #3450, 2.849999999999999201 ) ;
#12209 = PRODUCT ( 'circlip for shafts normal_din_Circlip DIN 471 - 7 x 0.8', 'circlip for shafts normal_din_Circlip DIN 471 - 7 x 0.8', '', ( #10065 ) ) ;
#12210 = AXIS2_PLACEMENT_3D ( 'NONE', #5661, #12471, #5460 ) ;
#12211 = EDGE_CURVE ( 'NONE', #9344, #5066, #12044, .T. ) ;
#12212 = LINE ( 'NONE', #8220, #6982 ) ;
#12213 = DIRECTION ( 'NONE',  ( 0.3090169943749492276, -0.9510565162951530871, 0.000000000000000000 ) ) ;
#12214 = DIRECTION ( 'NONE',  ( 0.000000000000000000, -0.000000000000000000, -1.000000000000000000 ) ) ;
#12215 = ORIENTED_EDGE ( 'NONE', *, *, #2897, .F. ) ;
#12216 = AXIS2_PLACEMENT_3D ( 'NONE', #11763, #2811, #3669 ) ;
#12217 = LINE ( 'NONE', #1151, #10349 ) ;
#12218 = CARTESIAN_POINT ( 'NONE',  ( 31.96709571323326671, 88.25314809233525182, 6.000000000000000000 ) ) ;
#12219 = AXIS2_PLACEMENT_3D ( 'NONE', #4095, #4157, #7157 ) ;
#12220 = ORIENTED_EDGE ( 'NONE', *, *, #11469, .F. ) ;
#12221 = FILL_AREA_STYLE_COLOUR ( '', #2169 ) ;
#12222 = DIRECTION ( 'NONE',  ( 0.000000000000000000, 0.000000000000000000, 1.000000000000000000 ) ) ;
#12223 = ORIENTED_EDGE ( 'NONE', *, *, #4725, .T. ) ;
#12224 = ORIENTED_EDGE ( 'NONE', *, *, #11898, .F. ) ;
#12225 = FACE_OUTER_BOUND ( 'NONE', #8896, .T. ) ;
#12226 = CARTESIAN_POINT ( 'NONE',  ( 64.47099661891824951, 100.7265662098817955, 2.755726390383620217 ) ) ;
#12227 = AXIS2_PLACEMENT_3D ( 'NONE', #2145, #5400, #6319 ) ;
#12228 = ORIENTED_EDGE ( 'NONE', *, *, #6632, .T. ) ;
#12229 = EDGE_CURVE ( 'NONE', #4495, #8808, #3093, .T. ) ;
#12230 = VECTOR ( 'NONE', #5289, 1000.000000000000000 ) ;
#12231 = ORIENTED_EDGE ( 'NONE', *, *, #7619, .T. ) ;
#12232 = DIRECTION ( 'NONE',  ( -1.000000000000000000, -0.000000000000000000, -0.000000000000000000 ) ) ;
#12233 = ORIENTED_EDGE ( 'NONE', *, *, #12239, .T. ) ;
#12234 = PRODUCT_CONTEXT ( 'NONE', #9009, 'mechanical' ) ;
#12235 = CARTESIAN_POINT ( 'NONE',  ( 35.00000000000000000, 126.3079067962035822, 2.890625000614516882 ) ) ;
#12236 = ORIENTED_EDGE ( 'NONE', *, *, #10835, .T. ) ;
#12237 = CIRCLE ( 'NONE', #11609, 30.19999999999999218 ) ;
#12238 = CARTESIAN_POINT ( 'NONE',  ( 30.00000000000000711, 2.000000000000001776, 1.500000000000000666 ) ) ;
#12239 = EDGE_CURVE ( 'NONE', #4447, #7980, #8201, .T. ) ;
#12240 = EDGE_LOOP ( 'NONE', ( #9353, #8170, #9593, #8140 ) ) ;
#12241 = EDGE_CURVE ( 'NONE', #9627, #4130, #7928, .T. ) ;
#12242 = AXIS2_PLACEMENT_3D ( 'NONE', #4173, #9264, #10048 ) ;
#12243 = DIRECTION ( 'NONE',  ( -0.000000000000000000, -0.000000000000000000, -1.000000000000000000 ) ) ;
#12244 = CARTESIAN_POINT ( 'NONE',  ( 66.19999999999998863, 90.00000000000000000, 3.537500001229034297 ) ) ;
#12245 = CARTESIAN_POINT ( 'NONE',  ( 66.20000000000000284, 71.98667160128370313, 3.500000001229034208 ) ) ;
#12246 = AXIS2_PLACEMENT_3D ( 'NONE', #12721, #7940, #5844 ) ;
#12247 = CARTESIAN_POINT ( 'NONE',  ( -4.763019983628629994, -4.349268977144818749, 0.000000000000000000 ) ) ;
#12248 = VERTEX_POINT ( 'NONE', #11915 ) ;
#12249 = VECTOR ( 'NONE', #12798, 1000.000000000000000 ) ;
#12250 = CARTESIAN_POINT ( 'NONE',  ( 66.20000000000000284, 71.98667160128370313, 3.837500000000000799 ) ) ;
#12251 = ORIENTED_EDGE ( 'NONE', *, *, #5108, .T. ) ;
#12252 = CARTESIAN_POINT ( 'NONE',  ( 19.40000000000000924, 117.0199925980744666, 3.125000000000000000 ) ) ;
#12253 = ORIENTED_EDGE ( 'NONE', *, *, #10546, .T. ) ;
#12254 = CARTESIAN_POINT ( 'NONE',  ( 3.800000000000015365, 90.00000000000000000, 3.650000000000000355 ) ) ;
#12255 = ORIENTED_EDGE ( 'NONE', *, *, #7635, .F. ) ;
#12256 = PRODUCT_DEFINITION ( 'UNKNOWN', '', #6348, #1232 ) ;
#12257 = CARTESIAN_POINT ( 'NONE',  ( -60.00000000000000000, 0.000000000000000000, 14.99999999999999645 ) ) ;
#12258 = CARTESIAN_POINT ( 'NONE',  ( 60.63303222545420823, 111.5086687406912347, 2.829484441871016109 ) ) ;
#12259 = VECTOR ( 'NONE', #12126, 1000.000000000000000 ) ;
#12260 = CARTESIAN_POINT ( 'NONE',  ( 66.44356964375000985, 71.84604660189820891, 3.696875000614517237 ) ) ;
#12261 = CARTESIAN_POINT ( 'NONE',  ( 25.00000000000000355, -5.000000000000000000, -7.250000000000000888 ) ) ;
#12262 = EDGE_CURVE ( 'NONE', #193, #5275, #6340, .T. ) ;
#12263 = DIRECTION ( 'NONE',  ( 1.000000000000000000, -0.000000000000000000, -0.000000000000000000 ) ) ;
#12264 = FACE_OUTER_BOUND ( 'NONE', #10239, .T. ) ;
#12265 = DIRECTION ( 'NONE',  ( 0.000000000000000000, 0.000000000000000000, 1.000000000000000000 ) ) ;
#12266 = DIRECTION ( 'NONE',  ( -0.000000000000000000, -0.000000000000000000, -1.000000000000000000 ) ) ;
#12267 = VECTOR ( 'NONE', #7893, 1000.000000000000000 ) ;
#12268 = DIRECTION ( 'NONE',  ( -0.000000000000000000, -1.000000000000000000, -0.000000000000000000 ) ) ;
#12269 = ADVANCED_FACE ( 'NONE', ( #915 ), #2960, .F. ) ;
#12270 = LINE ( 'NONE', #7296, #1042 ) ;
#12271 = CARTESIAN_POINT ( 'NONE',  ( 25.00000000000000355, 0.000000000000000000, -5.750000000000000000 ) ) ;
#12272 = ORIENTED_EDGE ( 'NONE', *, *, #9024, .T. ) ;
#12273 = DIRECTION ( 'NONE',  ( -0.000000000000000000, -0.000000000000000000, -1.000000000000000000 ) ) ;
#12274 = ORIENTED_EDGE ( 'NONE', *, *, #5274, .F. ) ;
#12275 = EDGE_CURVE ( 'NONE', #2032, #10118, #2978, .T. ) ;
#12276 = VECTOR ( 'NONE', #10436, 1000.000000000000000 ) ;
#12277 = SHAPE_REPRESENTATION_RELATIONSHIP ( 'NONE' , 'NONE' ,  #5503, #11356 ) ;
#12278 = CARTESIAN_POINT ( 'NONE',  ( 41.00904217445252442, 92.47818727009297390, 4.000000000000000000 ) ) ;
#12279 = CARTESIAN_POINT ( 'NONE',  ( 3.000000000000004441, 27.00000000000000000, 2.500000000000000000 ) ) ;
#12280 = DIRECTION ( 'NONE',  ( 1.000000000000000000, 0.000000000000000000, 0.000000000000000000 ) ) ;
#12281 = ORIENTED_EDGE ( 'NONE', *, *, #6543, .F. ) ;
#12282 = DIRECTION ( 'NONE',  ( -0.000000000000000000, -0.000000000000000000, -1.000000000000000000 ) ) ;
#12283 = DIRECTION ( 'NONE',  ( -0.000000000000000000, -0.000000000000000000, -1.000000000000000000 ) ) ;
#12284 = ORIENTED_EDGE ( 'NONE', *, *, #11517, .T. ) ;
#12285 = SHAPE_REPRESENTATION_RELATIONSHIP ( 'NONE' , 'NONE' ,  #4597, #1374 ) ;
#12286 = DIRECTION ( 'NONE',  ( -1.445602896647339656E-17, 0.000000000000000000, -1.000000000000000000 ) ) ;
#12287 = ORIENTED_EDGE ( 'NONE', *, *, #6114, .T. ) ;
#12288 = ADVANCED_FACE ( 'NONE', ( #3022, #7009, #1440, #1247, #381 ), #8319, .F. ) ;
#12289 = ORIENTED_EDGE ( 'NONE', *, *, #1409, .F. ) ;
#12290 = CARTESIAN_POINT ( 'NONE',  ( 7.650000000000000355, 0.000000000000000000, 0.000000000000000000 ) ) ;
#12291 = CARTESIAN_POINT ( 'NONE',  ( 36.50000000000001421, 67.79999999999999716, 8.000000000000000000 ) ) ;
#12292 = VECTOR ( 'NONE', #6846, 1000.000000000000000 ) ;
#12293 = ORIENTED_EDGE ( 'NONE', *, *, #10320, .T. ) ;
#12294 = VECTOR ( 'NONE', #1295, 1000.000000000000114 ) ;
#12295 = ORIENTED_EDGE ( 'NONE', *, *, #8076, .T. ) ;
#12296 = DIRECTION ( 'NONE',  ( 0.000000000000000000, -0.000000000000000000, 1.000000000000000000 ) ) ;
#12297 = VERTEX_POINT ( 'NONE', #5240 ) ;
#12298 = CARTESIAN_POINT ( 'NONE',  ( 66.44356964374999563, 90.00000000000000000, 3.678125000614516971 ) ) ;
#12299 = VERTEX_POINT ( 'NONE', #4392 ) ;
#12300 = CARTESIAN_POINT ( 'NONE',  ( -3.666666666666659413, 62.52406516434930239, 0.9999999999999991118 ) ) ;
#12301 = ORIENTED_EDGE ( 'NONE', *, *, #7427, .F. ) ;
#12302 = EDGE_CURVE ( 'NONE', #5275, #5282, #3266, .T. ) ;
#12303 = AXIS2_PLACEMENT_3D ( 'NONE', #5803, #8625, #10708 ) ;
#12304 = CARTESIAN_POINT ( 'NONE',  ( -60.00000000000000000, 30.00000000000000000, 7.999999999999996447 ) ) ;
#12305 = FACE_OUTER_BOUND ( 'NONE', #6076, .T. ) ;
#12306 = VECTOR ( 'NONE', #4017, 1000.000000000000114 ) ;
#12307 = CYLINDRICAL_SURFACE ( 'NONE', #12918, 6.499999999999999112 ) ;
#12308 = EDGE_CURVE ( 'NONE', #8376, #2989, #9440, .T. ) ;
#12309 = VECTOR ( 'NONE', #3502, 1000.000000000000000 ) ;
#12311 = EDGE_CURVE ( 'NONE', #12248, #39, #2307, .T. ) ;
#12310 = ORIENTED_EDGE ( 'NONE', *, *, #9909, .T. ) ;
#12312 = CARTESIAN_POINT ( 'NONE',  ( 50.72178482187499071, 117.2309300971526937, 4.259375000614517681 ) ) ;
#12313 = ORIENTED_EDGE ( 'NONE', *, *, #931, .T. ) ;
#12314 = LINE ( 'NONE', #2181, #11894 ) ;
#12315 = ORIENTED_EDGE ( 'NONE', *, *, #2114, .F. ) ;
#12316 = CARTESIAN_POINT ( 'NONE',  ( 50.60000000000001563, 62.98000740192552627, 3.800000000000000266 ) ) ;
#12317 = PRODUCT_DEFINITION_SHAPE ( 'NONE', 'NONE',  #10165 ) ;
#12318 = VERTEX_POINT ( 'NONE', #6147 ) ;
#12319 = CIRCLE ( 'NONE', #2717, 2.849999999999999201 ) ;
#12320 = CARTESIAN_POINT ( 'NONE',  ( 45.00000000000000000, -5.000000000000000000, -5.750000000000000000 ) ) ;
#12321 = EDGE_CURVE ( 'NONE', #10802, #7918, #2436, .T. ) ;
#12322 = DIRECTION ( 'NONE',  ( -0.000000000000000000, -1.000000000000000000, -0.000000000000000000 ) ) ;
#12323 = CARTESIAN_POINT ( 'NONE',  ( 64.54728993811707483, 100.7543353701752125, 2.858851390224067313 ) ) ;
#12324 = DIRECTION ( 'NONE',  ( 1.000000000000000000, 0.000000000000000000, 0.000000000000000000 ) ) ;
#12325 = FACE_OUTER_BOUND ( 'NONE', #12123, .T. ) ;
#12326 = CARTESIAN_POINT ( 'NONE',  ( 40.00000000000000000, 0.000000000000000000, -10.00000000000000000 ) ) ;
#12327 = VECTOR ( 'NONE', #6578, 1000.000000000000000 ) ;
#12328 = FACE_BOUND ( 'NONE', #5635, .T. ) ;
#12329 = FACE_OUTER_BOUND ( 'NONE', #6074, .T. ) ;
#12330 = LINE ( 'NONE', #9051, #1130 ) ;
#12331 = CARTESIAN_POINT ( 'NONE',  ( -60.00000000000000000, 30.00000000000000000, 3.000000000000000000 ) ) ;
#12332 = EDGE_CURVE ( 'NONE', #7638, #4183, #8386, .T. ) ;
#12333 = DIRECTION ( 'NONE',  ( 0.000000000000000000, 0.000000000000000000, 1.000000000000000000 ) ) ;
#12334 = DIRECTION ( 'NONE',  ( 1.000000000000000000, 0.000000000000000000, -0.000000000000000000 ) ) ;
#12335 = ORIENTED_EDGE ( 'NONE', *, *, #10397, .F. ) ;
#12336 = VECTOR ( 'NONE', #3971, 1000.000000000000227 ) ;
#12337 = CARTESIAN_POINT ( 'NONE',  ( 16.96438320935645905, 66.02675393316422969, -0.9999999999999970024 ) ) ;
#12338 = ORIENTED_EDGE ( 'NONE', *, *, #11563, .F. ) ;
#12339 = AXIS2_PLACEMENT_3D ( 'NONE', #7836, #10714, #887 ) ;
#12340 = SURFACE_STYLE_USAGE ( .BOTH. , #9195 ) ;
#12341 = DIRECTION ( 'NONE',  ( -0.000000000000000000, 1.000000000000000000, -0.000000000000000000 ) ) ;
#12342 = CARTESIAN_POINT ( 'NONE',  ( 0.000000000000000000, 0.000000000000000000, -10.00000000000000000 ) ) ;
#12343 = CARTESIAN_POINT ( 'NONE',  ( 35.75000000000000711, 93.41869858279433458, -3.799999999999999378 ) ) ;
#12344 = VECTOR ( 'NONE', #10356, 1000.000000000000000 ) ;
#12345 = ORIENTED_EDGE ( 'NONE', *, *, #10397, .T. ) ;
#12346 = CARTESIAN_POINT ( 'NONE',  ( -0.9999999999999997780, -4.273461295629625845, 0.000000000000000000 ) ) ;
#12347 = EDGE_CURVE ( 'NONE', #11778, #10533, #9446, .T. ) ;
#12348 = CARTESIAN_POINT ( 'NONE',  ( -67.46410161513773573, 36.92820323027551410, -2.500000000000000000 ) ) ;
#12349 = ORIENTED_EDGE ( 'NONE', *, *, #8879, .F. ) ;
#12350 = CARTESIAN_POINT ( 'NONE',  ( 0.000000000000000000, 0.000000000000000000, 0.000000000000000000 ) ) ;
#12351 = CARTESIAN_POINT ( 'NONE',  ( -23.49999999999999289, 53.38268590218009280, 1.000000000000000000 ) ) ;
#12352 = ORIENTED_EDGE ( 'NONE', *, *, #10102, .T. ) ;
#12353 = VERTEX_POINT ( 'NONE', #12244 ) ;
#12354 = DIRECTION ( 'NONE',  ( 0.000000000000000000, -1.000000000000000000, -0.000000000000000000 ) ) ;
#12355 = CARTESIAN_POINT ( 'NONE',  ( -60.00000000000000000, -6.000000000000000000, 14.99999999999999645 ) ) ;
#12356 = ORIENTED_EDGE ( 'NONE', *, *, #10227, .F. ) ;
#12357 = EDGE_CURVE ( 'NONE', #6585, #7921, #5472, .T. ) ;
#12358 = ORIENTED_EDGE ( 'NONE', *, *, #9746, .F. ) ;
#12359 = DIRECTION ( 'NONE',  ( 0.000000000000000000, 1.000000000000000000, 1.224646799147353207E-16 ) ) ;
#12360 = EDGE_LOOP ( 'NONE', ( #1312, #378, #4948, #7061 ) ) ;
#12361 = FACE_BOUND ( 'NONE', #4316, .T. ) ;
#12362 = ADVANCED_FACE ( 'NONE', ( #10142 ), #7269, .F. ) ;
#12363 = CARTESIAN_POINT ( 'NONE',  ( 50.59999999999999432, 117.0199925980744666, 3.612500001229034474 ) ) ;
#12364 = ORIENTED_EDGE ( 'NONE', *, *, #1518, .T. ) ;
#12365 = APPLICATION_CONTEXT ( 'automotive_design' ) ;
#12366 = FACE_OUTER_BOUND ( 'NONE', #1158, .T. ) ;
#12367 = EDGE_LOOP ( 'NONE', ( #5160, #2944, #12739, #1420 ) ) ;
#12368 = CARTESIAN_POINT ( 'NONE',  ( 0.000000000000000000, 1.154700538379252350, 7.017607234860990640E-28 ) ) ;
#12369 = CARTESIAN_POINT ( 'NONE',  ( 1.000000000000000000, -5.473461295629626022, -0.8000000000000000444 ) ) ;
#12370 = PLANE ( 'NONE',  #6636 ) ;
#12371 = AXIS2_PLACEMENT_3D ( 'NONE', #6554, #788, #5771 ) ;
#12372 = EDGE_CURVE ( 'NONE', #1569, #10050, #7148, .T. ) ;
#12373 = ORIENTED_EDGE ( 'NONE', *, *, #9583, .F. ) ;
#12374 = FACE_OUTER_BOUND ( 'NONE', #8024, .T. ) ;
#12375 = EDGE_LOOP ( 'NONE', ( #9914, #9610, #962, #11029 ) ) ;
#12376 = CARTESIAN_POINT ( 'NONE',  ( 50.00000000000000000, 121.2009999999999934, 1.500000000000001332 ) ) ;
#12377 = CARTESIAN_POINT ( 'NONE',  ( 50.72178482187499071, 117.2309300971526937, 4.259375000614517681 ) ) ;
#12378 = ORIENTED_EDGE ( 'NONE', *, *, #867, .T. ) ;
#12379 = VECTOR ( 'NONE', #9936, 1000.000000000000227 ) ;
#12380 = CARTESIAN_POINT ( 'NONE',  ( 8.500000000000000000, 71.85789451624832225, 2.999999999999919620 ) ) ;
#12381 = DIRECTION ( 'NONE',  ( 0.000000000000000000, 0.000000000000000000, 1.000000000000000000 ) ) ;
#12382 = CARTESIAN_POINT ( 'NONE',  ( 50.72178482187501203, 62.76906990284730625, 4.559375000614517504 ) ) ;
#12383 = DIRECTION ( 'NONE',  ( 0.000000000000000000, -1.000000000000000000, 0.000000000000000000 ) ) ;
#12384 = DIRECTION ( 'NONE',  ( 0.000000000000000000, 0.000000000000000000, 1.000000000000000000 ) ) ;
#12385 = LINE ( 'NONE', #1460, #7302 ) ;
#12386 = PLANE ( 'NONE',  #5102 ) ;
#12387 = ADVANCED_FACE ( 'NONE', ( #6343, #5427 ), #4328, .F. ) ;
#12388 = CARTESIAN_POINT ( 'NONE',  ( -28.99038105676692112, 50.21281292110204930, 1.000000000000000000 ) ) ;
#12389 = DIRECTION ( 'NONE',  ( 1.000000000000000000, 0.000000000000000000, 0.000000000000000000 ) ) ;
#12390 = AXIS2_PLACEMENT_3D ( 'NONE', #10026, #5439, #8523 ) ;
#12391 = DIRECTION ( 'NONE',  ( -0.000000000000000000, 1.000000000000000000, -0.000000000000000000 ) ) ;
#12392 = CARTESIAN_POINT ( 'NONE',  ( 19.40000000000000924, 117.0199925980744666, 4.924999999999999822 ) ) ;
#12393 = CARTESIAN_POINT ( 'NONE',  ( -56.80384757729341771, 34.46410161513777837, 0.000000000000000000 ) ) ;
#12395 = ADVANCED_FACE ( 'NONE', ( #4455 ), #5171, .F. ) ;
#12394 = ORIENTED_EDGE ( 'NONE', *, *, #4550, .T. ) ;
#12396 = EDGE_CURVE ( 'NONE', #7515, #2123, #8188, .T. ) ;
#12397 = CARTESIAN_POINT ( 'NONE',  ( -0.1038759689922479496, -3.348389132562988646, -0.8000000000000000444 ) ) ;
#12398 = DIRECTION ( 'NONE',  ( -1.000000000000000000, -0.000000000000000000, -0.000000000000000000 ) ) ;
#12399 = VERTEX_POINT ( 'NONE', #10602 ) ;
#12400 = AXIS2_PLACEMENT_3D ( 'NONE', #12148, #10112, #12280 ) ;
#12401 = PLANE ( 'NONE',  #11583 ) ;
#12402 = DIRECTION ( 'NONE',  ( 0.000000000000000000, -0.000000000000000000, 1.000000000000000000 ) ) ;
#12403 = DIRECTION ( 'NONE',  ( -1.000000000000000000, -0.000000000000000000, -0.000000000000000000 ) ) ;
#12404 = AXIS2_PLACEMENT_3D ( 'NONE', #10512, #1547, #5403 ) ;
#12405 = ORIENTED_EDGE ( 'NONE', *, *, #3482, .F. ) ;
#12406 = CARTESIAN_POINT ( 'NONE',  ( 1.040000000000000036, -1.154700538379251684, 0.000000000000000000 ) ) ;
#12407 = DIRECTION ( 'NONE',  ( 0.03100775193798452692, -0.9995191440486532741, 0.000000000000000000 ) ) ;
#12408 = ORIENTED_EDGE ( 'NONE', *, *, #12730, .T. ) ;
#12409 = CARTESIAN_POINT ( 'NONE',  ( 0.000000000000000000, 0.000000000000000000, 0.000000000000000000 ) ) ;
#12410 = VECTOR ( 'NONE', #4175, 1000.000000000000000 ) ;
#12411 = DIRECTION ( 'NONE',  ( 0.000000000000000000, 0.000000000000000000, 1.000000000000000000 ) ) ;
#12412 = VERTEX_POINT ( 'NONE', #6476 ) ;
#12413 = VECTOR ( 'NONE', #10633, 1000.000000000000000 ) ;
#12414 = CARTESIAN_POINT ( 'NONE',  ( 35.00000000000000000, 90.00000000000000000, 4.000000000000000000 ) ) ;
#12415 = EDGE_LOOP ( 'NONE', ( #11109, #2084 ) ) ;
#12416 = LINE ( 'NONE', #630, #11548 ) ;
#12417 = DIRECTION ( 'NONE',  ( -1.000000000000000000, 0.000000000000000000, 0.000000000000000000 ) ) ;
#12418 = EDGE_CURVE ( 'NONE', #2970, #10857, #3739, .T. ) ;
#12419 = ORIENTED_EDGE ( 'NONE', *, *, #10120, .F. ) ;
#12420 = AXIS2_PLACEMENT_3D ( 'NONE', #11874, #12858, #12792 ) ;
#12421 = PRODUCT_DEFINITION_SHAPE ( 'NONE', 'NONE',  #2349 ) ;
#12422 = FACE_OUTER_BOUND ( 'NONE', #6475, .T. ) ;
#12423 = AXIS2_PLACEMENT_3D ( 'NONE', #9638, #535, #7419 ) ;
#12424 =( BOUNDED_CURVE ( )  B_SPLINE_CURVE ( 2, ( #6444, #1476, #9828, #12540, #5461, #8485, #856 ),
 .UNSPECIFIED., .F., .F. ) 
 B_SPLINE_CURVE_WITH_KNOTS ( ( 3, 2, 2, 3 ),
 ( 0.1000000000000001860, 0.1333333333333334425, 0.1666666666666666852, 0.2000000000000000111 ),
 .UNSPECIFIED. ) 
 CURVE ( )  GEOMETRIC_REPRESENTATION_ITEM ( )  RATIONAL_B_SPLINE_CURVE ( ( 0.9999999999999992228, 0.8660254037844394848, 1.000000000000000000, 0.8660254037844387076, 1.000000000000000000, 0.8660254037844388186, 0.9999999999999998890 ) ) 
 REPRESENTATION_ITEM ( '' )  );
#12425 = DIRECTION ( 'NONE',  ( -0.3262398754384822630, 0.9452870165584014162, 0.000000000000000000 ) ) ;
#12426 = ORIENTED_EDGE ( 'NONE', *, *, #5188, .F. ) ;
#12427 = CARTESIAN_POINT ( 'NONE',  ( 47.03610297002379781, 118.9238557598572896, 3.000000000000000444 ) ) ;
#12428 = CONTEXT_DEPENDENT_SHAPE_REPRESENTATION ( #12114, #7223 ) ;
#12429 = CARTESIAN_POINT ( 'NONE',  ( 3.800000000000015365, 90.00000000000000000, 4.662500001229034297 ) ) ;
#12430 = EDGE_LOOP ( 'NONE', ( #10002, #5895, #11325, #3273, #5286 ) ) ;
#12431 = PRESENTATION_STYLE_ASSIGNMENT (( #643 ) ) ;
#12432 = ORIENTED_EDGE ( 'NONE', *, *, #12433, .T. ) ;
#12433 = EDGE_CURVE ( 'NONE', #10547, #3551, #7783, .T. ) ;
#12434 = DIRECTION ( 'NONE',  ( 0.000000000000000000, 0.000000000000000000, 1.000000000000000000 ) ) ;
#12436 = ORIENTED_EDGE ( 'NONE', *, *, #5039, .F. ) ;
#12435 = VECTOR ( 'NONE', #8788, 1000.000000000000000 ) ;
#12437 = VECTOR ( 'NONE', #9874, 1000.000000000000227 ) ;
#12438 = CARTESIAN_POINT ( 'NONE',  ( 50.59999999999999432, 117.0199925980744666, 3.162500001229034741 ) ) ;
#12439 = DIRECTION ( 'NONE',  ( 0.000000000000000000, 0.000000000000000000, -1.000000000000000000 ) ) ;
#12440 = EDGE_CURVE ( 'NONE', #12799, #12605, #9671, .T. ) ;
#12441 = ORIENTED_EDGE ( 'NONE', *, *, #11078, .F. ) ;
#12442 = CARTESIAN_POINT ( 'NONE',  ( 19.40000000000002700, 62.98000740192551206, 4.287500001229034297 ) ) ;
#12443 = AXIS2_PLACEMENT_3D ( 'NONE', #10966, #9070, #8942 ) ;
#12444 = CARTESIAN_POINT ( 'NONE',  ( -15.06519709809452756, 92.38262548349219117, 1.000000000000003109 ) ) ;
#12445 = AXIS2_PLACEMENT_3D ( 'NONE', #2551, #12296, #6529 ) ;
#12446 = VERTEX_POINT ( 'NONE', #11515 ) ;
#12447 = LINE ( 'NONE', #4532, #4257 ) ;
#12448 = ORIENTED_EDGE ( 'NONE', *, *, #5266, .T. ) ;
#12449 = CARTESIAN_POINT ( 'NONE',  ( -48.33333333333332860, 2.000000000000000000, 1.599999999999992095 ) ) ;
#12450 = DIRECTION ( 'NONE',  ( 1.000000000000000000, 0.000000000000000000, 0.000000000000000000 ) ) ;
#12451 = EDGE_CURVE ( 'NONE', #12152, #4194, #2779, .T. ) ;
#12452 = CARTESIAN_POINT ( 'NONE',  ( 35.00000000000000000, 126.3079067962036106, 3.396875000614517415 ) ) ;
#12453 = LINE ( 'NONE', #11598, #9146 ) ;
#12454 = AXIS2_PLACEMENT_3D ( 'NONE', #6045, #11015, #10039 ) ;
#12455 = CARTESIAN_POINT ( 'NONE',  ( 0.000000000000000000, 0.000000000000000000, -0.8000000000000000444 ) ) ;
#12456 = VECTOR ( 'NONE', #3582, 1000.000000000000114 ) ;
#12457 = LINE ( 'NONE', #7352, #5408 ) ;
#12458 = CARTESIAN_POINT ( 'NONE',  ( 45.00000000000000000, -5.000000000000000000, -5.750000000000000000 ) ) ;
#12459 = CARTESIAN_POINT ( 'NONE',  ( 66.20000000000000284, 90.00000000000000000, 3.000000000000000000 ) ) ;
#12460 = DIRECTION ( 'NONE',  ( -1.000000000000000000, -0.000000000000000000, -0.000000000000000000 ) ) ;
#12461 = PLANE ( 'NONE',  #10575 ) ;
#12462 = VECTOR ( 'NONE', #1156, 1000.000000000000000 ) ;
#12463 = CARTESIAN_POINT ( 'NONE',  ( 52.45028081366923089, 66.83239978927284142, 0.6666666666666665186 ) ) ;
#12464 = PLANE ( 'NONE',  #11207 ) ;
#12465 = ORIENTED_EDGE ( 'NONE', *, *, #6976, .F. ) ;
#12466 = EDGE_CURVE ( 'NONE', #1104, #6338, #10913, .T. ) ;
#12467 = DIRECTION ( 'NONE',  ( 1.000000000000000000, 0.000000000000000000, 0.000000000000000000 ) ) ;
#12468 = CARTESIAN_POINT ( 'NONE',  ( 65.19999999999998863, 90.00000000000000000, -5.000000000000000000 ) ) ;
#12469 = EDGE_LOOP ( 'NONE', ( #3320, #11981, #328, #2072, #355, #11371 ) ) ;
#12470 = CIRCLE ( 'NONE', #3906, 6.499999999999999112 ) ;
#12471 = DIRECTION ( 'NONE',  ( -0.000000000000000000, -0.000000000000000000, -1.000000000000000000 ) ) ;
#12472 = DIRECTION ( 'NONE',  ( 0.000000000000000000, -0.000000000000000000, 1.000000000000000000 ) ) ;
#12473 = ADVANCED_FACE ( 'NONE', ( #10662 ), #4653, .T. ) ;
#12474 = DIRECTION ( 'NONE',  ( -0.000000000000000000, -1.000000000000000000, -0.000000000000000000 ) ) ;
#12475 = EDGE_CURVE ( 'NONE', #7686, #108, #12620, .T. ) ;
#12476 = ORIENTED_EDGE ( 'NONE', *, *, #12347, .F. ) ;
#12477 = CARTESIAN_POINT ( 'NONE',  ( 1.436050757534458100, -5.516136167806656943, 0.000000000000000000 ) ) ;
#12478 = CARTESIAN_POINT ( 'NONE',  ( 3.000000000000004441, 30.00000000000000000, 8.000000000000000000 ) ) ;
#12479 = ORIENTED_EDGE ( 'NONE', *, *, #7923, .F. ) ;
#12480 = CARTESIAN_POINT ( 'NONE',  ( 0.000000000000000000, 0.000000000000000000, 0.000000000000000000 ) ) ;
#12481 = DIRECTION ( 'NONE',  ( -0.000000000000000000, -0.000000000000000000, 1.000000000000000000 ) ) ;
#12482 = ORIENTED_EDGE ( 'NONE', *, *, #895, .F. ) ;
#12483 = CIRCLE ( 'NONE', #3914, 1.599999999999986766 ) ;
#12484 = LINE ( 'NONE', #11687, #5365 ) ;
#12485 = ORIENTED_EDGE ( 'NONE', *, *, #3228, .F. ) ;
#12486 = EDGE_CURVE ( 'NONE', #2419, #11257, #4904, .T. ) ;
#12487 = CARTESIAN_POINT ( 'NONE',  ( 25.00000000000000355, 0.000000000000000000, 5.750000000000000000 ) ) ;
#12488 = DIRECTION ( 'NONE',  ( 1.000000000000000000, 0.000000000000000000, 2.891205793294678696E-17 ) ) ;
#12489 = ORIENTED_EDGE ( 'NONE', *, *, #6577, .F. ) ;
#12490 = ORIENTED_EDGE ( 'NONE', *, *, #8366, .T. ) ;
#12491 = AXIS2_PLACEMENT_3D ( 'NONE', #11737, #4027, #6895 ) ;
#12492 = DIRECTION ( 'NONE',  ( -0.000000000000000000, -0.000000000000000000, -1.000000000000000000 ) ) ;
#12493 = PRODUCT_RELATED_PRODUCT_CATEGORY ( 'part', '', ( #1339 ) ) ;
#12494 = ORIENTED_EDGE ( 'NONE', *, *, #12262, .T. ) ;
#12495 = LINE ( 'NONE', #3538, #10341 ) ;
#12496 = ITEM_DEFINED_TRANSFORMATION ( 'NONE', 'NONE', #1969,  #5704 ) ;
#12497 = DIRECTION ( 'NONE',  ( -0.000000000000000000, -0.000000000000000000, -1.000000000000000000 ) ) ;
#12498 = ORIENTED_EDGE ( 'NONE', *, *, #11705, .T. ) ;
#12499 = ADVANCED_FACE ( 'NONE', ( #10000 ), #3076, .T. ) ;
#12500 = DIRECTION ( 'NONE',  ( 0.000000000000000000, 0.000000000000000000, -1.000000000000000000 ) ) ;
#12501 = ORIENTED_EDGE ( 'NONE', *, *, #5678, .T. ) ;
#12502 = ORIENTED_EDGE ( 'NONE', *, *, #7200, .T. ) ;
#12503 = AXIS2_PLACEMENT_3D ( 'NONE', #8692, #635, #12683 ) ;
#12504 = VECTOR ( 'NONE', #12519, 1000.000000000000000 ) ;
#12505 = DIRECTION ( 'NONE',  ( 0.4719909656437444867, -0.8816033849473842166, 0.000000000000000000 ) ) ;
#12506 = FACE_BOUND ( 'NONE', #8894, .T. ) ;
#12507 = ORIENTED_EDGE ( 'NONE', *, *, #11121, .T. ) ;
#12508 = DIRECTION ( 'NONE',  ( 0.000000000000000000, 0.000000000000000000, 1.000000000000000000 ) ) ;
#12509 = ORIENTED_EDGE ( 'NONE', *, *, #9492, .T. ) ;
#12510 = CARTESIAN_POINT ( 'NONE',  ( 19.40000000000002700, 62.98000740192551206, 2.937500001229034208 ) ) ;
#12511 = VECTOR ( 'NONE', #7122, 1000.000000000000000 ) ;
#12512 = VERTEX_POINT ( 'NONE', #966 ) ;
#12513 = CARTESIAN_POINT ( 'NONE',  ( 35.00000000000000000, 126.3079067962035822, 3.846875000614517592 ) ) ;
#12514 = EDGE_CURVE ( 'NONE', #5455, #9206, #10075, .T. ) ;
#12515 = ORIENTED_EDGE ( 'NONE', *, *, #3328, .F. ) ;
#12516 = DIRECTION ( 'NONE',  ( 1.301042606982605321E-15, 0.000000000000000000, 1.000000000000000000 ) ) ;
#12517 = CARTESIAN_POINT ( 'NONE',  ( 51.63935276957964504, 66.24642824321904300, 4.000000000000000000 ) ) ;
#12518 = DIRECTION ( 'NONE',  ( 0.000000000000000000, 0.000000000000000000, -1.000000000000000000 ) ) ;
#12519 = DIRECTION ( 'NONE',  ( 0.000000000000000000, 1.000000000000000000, 0.000000000000000000 ) ) ;
#12521 = CYLINDRICAL_SURFACE ( 'NONE', #11037, 6.450000000000001066 ) ;
#12520 = VECTOR ( 'NONE', #3153, 1000.000000000000000 ) ;
#12522 = FACE_OUTER_BOUND ( 'NONE', #4898, .T. ) ;
#12523 = CARTESIAN_POINT ( 'NONE',  ( 12.55092940903992194, 109.9007343985615393, 1.000000000000003553 ) ) ;
#12524 = EDGE_CURVE ( 'NONE', #12851, #9926, #2368, .T. ) ;
#12525 = CARTESIAN_POINT ( 'NONE',  ( 31.50000000000000711, 90.00000000000000000, -3.000000000000000000 ) ) ;
#12526 = DIRECTION ( 'NONE',  ( -0.000000000000000000, -0.000000000000000000, -1.000000000000000000 ) ) ;
#12527 = AXIS2_PLACEMENT_3D ( 'NONE', #2764, #3874, #5825 ) ;
#12528 = PLANE ( 'NONE',  #4098 ) ;
#12529 = EDGE_CURVE ( 'NONE', #7127, #9471, #37, .T. ) ;
#12530 = AXIS2_PLACEMENT_3D ( 'NONE', #3756, #11854, #7738 ) ;
#12531 = LINE ( 'NONE', #9771, #11499 ) ;
#12532 = CARTESIAN_POINT ( 'NONE',  ( 1.750000000000000000, 0.000000000000000000, 0.000000000000000000 ) ) ;
#12533 = VERTEX_POINT ( 'NONE', #897 ) ;
#12534 = LINE ( 'NONE', #4116, #10277 ) ;
#12535 = CARTESIAN_POINT ( 'NONE',  ( 35.00000000000000000, 90.00000000000000000, -18.00000000000000355 ) ) ;
#12536 = ORIENTED_EDGE ( 'NONE', *, *, #6705, .T. ) ;
#12537 = SURFACE_STYLE_FILL_AREA ( #10501 ) ;
#12538 = CIRCLE ( 'NONE', #5206, 1.500000000000000222 ) ;
#12539 = LINE ( 'NONE', #480, #1770 ) ;
#12540 = CARTESIAN_POINT ( 'NONE',  ( 35.00000000000000711, 53.97334320256736362, 4.662499999999999645 ) ) ;
#12541 = APPLICATION_CONTEXT ( 'automotive_design' ) ;
#12542 = ADVANCED_FACE ( 'NONE', ( #2885 ), #4841, .T. ) ;
#12543 = CARTESIAN_POINT ( 'NONE',  ( 38.50000000000000711, 90.00000000000000000, 6.000000000000000000 ) ) ;
#12544 = ORIENTED_EDGE ( 'NONE', *, *, #1803, .T. ) ;
#12545 = CARTESIAN_POINT ( 'NONE',  ( 30.00000000000000711, 2.000000000000000000, 10.00000000000000000 ) ) ;
#12546 = DIRECTION ( 'NONE',  ( 0.000000000000000000, 0.000000000000000000, 1.000000000000000000 ) ) ;
#12547 = ORIENTED_EDGE ( 'NONE', *, *, #9870, .F. ) ;
#12548 = CIRCLE ( 'NONE', #1257, 3.500000000000003109 ) ;
#12549 = EDGE_CURVE ( 'NONE', #10547, #11451, #11899, .T. ) ;
#12550 =( NAMED_UNIT ( * ) SI_UNIT ( $, .STERADIAN. ) SOLID_ANGLE_UNIT ( ) );
#12551 =( NAMED_UNIT ( * ) PLANE_ANGLE_UNIT ( ) SI_UNIT ( $, .RADIAN. ) );
#12552 = ORIENTED_EDGE ( 'NONE', *, *, #3804, .T. ) ;
#12553 = PLANE ( 'NONE',  #8918 ) ;
#12554 = ORIENTED_EDGE ( 'NONE', *, *, #12920, .T. ) ;
#12555 = EDGE_CURVE ( 'NONE', #12562, #9627, #9030, .T. ) ;
#12556 = DIRECTION ( 'NONE',  ( -0.000000000000000000, -0.000000000000000000, -1.000000000000000000 ) ) ;
#12557 = DIRECTION ( 'NONE',  ( 0.4719909656437442647, -0.8816033849473842166, 2.775557561595757269E-17 ) ) ;
#12558 = CONICAL_SURFACE ( 'NONE', #410, 1732.050807568857181, 1.047197551196592746 ) ;
#12559 = DIRECTION ( 'NONE',  ( 0.000000000000000000, 0.000000000000000000, 1.000000000000000000 ) ) ;
#12560 = CARTESIAN_POINT ( 'NONE',  ( 0.000000000000000000, 0.000000000000000000, -0.8000000000000000444 ) ) ;
#12561 = DIRECTION ( 'NONE',  ( -0.9510565162951529761, -0.3090169943749492276, 0.000000000000000000 ) ) ;
#12562 = VERTEX_POINT ( 'NONE', #10059 ) ;
#12563 = CARTESIAN_POINT ( 'NONE',  ( 0.000000000000000000, 0.000000000000000000, 0.000000000000000000 ) ) ;
#12564 = CARTESIAN_POINT ( 'NONE',  ( 60.43447243729646345, 111.3420572890634048, 2.688859442485532991 ) ) ;
#12565 = EDGE_LOOP ( 'NONE', ( #5786, #11134, #9789, #11991 ) ) ;
#12566 = PLANE ( 'NONE',  #105 ) ;
#12567 = ORIENTED_EDGE ( 'NONE', *, *, #10241, .T. ) ;
#12568 = CIRCLE ( 'NONE', #6909, 1.500000000000000222 ) ;
#12569 = FILL_AREA_STYLE_COLOUR ( '', #8809 ) ;
#12570 = ORIENTED_EDGE ( 'NONE', *, *, #2926, .F. ) ;
#12571 = ADVANCED_FACE ( 'NONE', ( #6926 ), #10910, .T. ) ;
#12572 = ADVANCED_FACE ( 'NONE', ( #6988, #5085, #3006 ), #4118, .T. ) ;
#12573 = CARTESIAN_POINT ( 'NONE',  ( 8.822182765162120077, 72.71083356296912825, 3.000000000000001776 ) ) ;
#12574 = LINE ( 'NONE', #5493, #2273 ) ;
#12575 = VERTEX_POINT ( 'NONE', #1895 ) ;
#12576 = VECTOR ( 'NONE', #1973, 1000.000000000000114 ) ;
#12577 = CARTESIAN_POINT ( 'NONE',  ( 19.27821517812500574, 117.2309300971526937, 2.984375000614517326 ) ) ;
#12578 = VERTEX_POINT ( 'NONE', #8892 ) ;
#12579 = CARTESIAN_POINT ( 'NONE',  ( 66.20000000000008811, 108.0133283987162542, 3.125000001229034208 ) ) ;
#12580 = VERTEX_POINT ( 'NONE', #3932 ) ;
#12581 = CARTESIAN_POINT ( 'NONE',  ( 35.00000000000000711, 53.69209320379640360, 4.071875000614516793 ) ) ;
#12582 = ORIENTED_EDGE ( 'NONE', *, *, #1437, .F. ) ;
#12583 = DIRECTION ( 'NONE',  ( -0.3090169943749500048, 0.9510565162951528650, 0.000000000000000000 ) ) ;
#12584 = CARTESIAN_POINT ( 'NONE',  ( -60.00000000000000000, 30.00000000000000000, 1.000000000000000000 ) ) ;
#12585 = DIRECTION ( 'NONE',  ( 0.000000000000000000, 0.000000000000000000, 1.000000000000000000 ) ) ;
#12586 = PRODUCT_DEFINITION ( 'UNKNOWN', '', #7401, #5412 ) ;
#12587 = DIRECTION ( 'NONE',  ( 0.000000000000000000, 0.000000000000000000, 1.000000000000000000 ) ) ;
#12588 = CARTESIAN_POINT ( 'NONE',  ( 66.20000000000000284, 90.00000000000000000, 6.000000000000000000 ) ) ;
#12589 = EDGE_CURVE ( 'NONE', #12297, #11127, #6798, .T. ) ;
#12590 = DIRECTION ( 'NONE',  ( 0.000000000000000000, 0.000000000000000000, 1.000000000000000000 ) ) ;
#12591 = DIRECTION ( 'NONE',  ( 5.337610695313252124E-17, 0.000000000000000000, -1.000000000000000000 ) ) ;
#12592 = CARTESIAN_POINT ( 'NONE',  ( 1.649999999999999023, 0.000000000000000000, 1.599999999999998757 ) ) ;
#12593 = FACE_OUTER_BOUND ( 'NONE', #6737, .T. ) ;
#12594 = CARTESIAN_POINT ( 'NONE',  ( 45.00000000000000000, -5.000000000000000000, -5.750000000000000000 ) ) ;
#12595 = DIRECTION ( 'NONE',  ( 0.000000000000000000, 0.000000000000000000, 1.000000000000000000 ) ) ;
#12596 = EDGE_LOOP ( 'NONE', ( #5093, #5244, #2216, #6051, #3639, #4966, #11579, #9998, #4773, #10279, #6133, #315, #6005, #7264, #3196, #2255, #2867, #5873, #6318, #6231 ) ) ;
#12597 = CARTESIAN_POINT ( 'NONE',  ( 19.40000000000000924, 117.0199925980744666, 4.924999999999999822 ) ) ;
#12598 = CARTESIAN_POINT ( 'NONE',  ( -60.00000000000000000, 0.000000000000000000, 9.999999999999996447 ) ) ;
#12599 = VERTEX_POINT ( 'NONE', #5026 ) ;
#12600 = EDGE_CURVE ( 'NONE', #6886, #7310, #4445, .T. ) ;
#12601 = CIRCLE ( 'NONE', #2148, 3.500000000000003109 ) ;
#12602 = EDGE_CURVE ( 'NONE', #2398, #10844, #4964, .T. ) ;
#12603 = DIRECTION ( 'NONE',  ( 0.000000000000000000, -1.000000000000000000, 0.000000000000000000 ) ) ;
#12604 = PLANE ( 'NONE',  #490 ) ;
#12605 = VERTEX_POINT ( 'NONE', #3993 ) ;
#12606 = PLANE ( 'NONE',  #91 ) ;
#12607 = CARTESIAN_POINT ( 'NONE',  ( 66.44356964375000985, 71.84604660189820891, 3.190625000614517592 ) ) ;
#12608 = VERTEX_POINT ( 'NONE', #7977 ) ;
#12609 =( GEOMETRIC_REPRESENTATION_CONTEXT ( 3 ) GLOBAL_UNCERTAINTY_ASSIGNED_CONTEXT ( ( #9490 ) ) GLOBAL_UNIT_ASSIGNED_CONTEXT ( ( #9260, #2276, #4169 ) ) REPRESENTATION_CONTEXT ( 'NONE', 'WORKASPACE' ) );
#12610 = CARTESIAN_POINT ( 'NONE',  ( -38.66666666666665719, 46.12451549659709116, -7.999999999999996447 ) ) ;
#12611 = DIRECTION ( 'NONE',  ( 0.000000000000000000, 0.000000000000000000, -1.000000000000000000 ) ) ;
#12612 = ORIENTED_EDGE ( 'NONE', *, *, #8720, .F. ) ;
#12613 = CARTESIAN_POINT ( 'NONE',  ( 66.19999999999998863, 90.00000000000000000, 4.325000000000000178 ) ) ;
#12614 = ORIENTED_EDGE ( 'NONE', *, *, #7283, .T. ) ;
#12615 = CIRCLE ( 'NONE', #1320, 28.99999999999999289 ) ;
#12616 = ADVANCED_FACE ( 'NONE', ( #1031 ), #11960, .F. ) ;
#12617 = DIRECTION ( 'NONE',  ( 0.000000000000000000, 0.000000000000000000, 1.000000000000000000 ) ) ;
#12618 = DIRECTION ( 'NONE',  ( -5.624500927088228034E-17, 1.370729058197317775E-18, 1.000000000000000000 ) ) ;
#12619 =( GEOMETRIC_REPRESENTATION_CONTEXT ( 3 ) GLOBAL_UNCERTAINTY_ASSIGNED_CONTEXT ( ( #9623 ) ) GLOBAL_UNIT_ASSIGNED_CONTEXT ( ( #10017, #6767, #2788 ) ) REPRESENTATION_CONTEXT ( 'NONE', 'WORKASPACE' ) );
#12620 =( BOUNDED_CURVE ( )  B_SPLINE_CURVE ( 2, ( #5693, #514, #5562, #12028, #6003, #9868, #4054 ),
 .UNSPECIFIED., .F., .F. ) 
 B_SPLINE_CURVE_WITH_KNOTS ( ( 3, 2, 2, 3 ),
 ( 0.3000000000000002109, 0.3333333333333334259, 0.3666666666666666963, 0.3999999999999999667 ),
 .UNSPECIFIED. ) 
 CURVE ( )  GEOMETRIC_REPRESENTATION_ITEM ( )  RATIONAL_B_SPLINE_CURVE ( ( 0.9999999999999991118, 0.8660254037844395958, 1.000000000000000000, 0.8660254037844387076, 1.000000000000000000, 0.8660254037844389297, 0.9999999999999997780 ) ) 
 REPRESENTATION_ITEM ( '' )  );
#12621 = LINE ( 'NONE', #2677, #2060 ) ;
#12622 = DIRECTION ( 'NONE',  ( 0.000000000000000000, 0.000000000000000000, 1.000000000000000000 ) ) ;
#12623 = DIRECTION ( 'NONE',  ( 1.000000000000000000, 0.000000000000000000, 2.891205793294678696E-17 ) ) ;
#12624 = VERTEX_POINT ( 'NONE', #1421 ) ;
#12625 = AXIS2_PLACEMENT_3D ( 'NONE', #8878, #6977, #3919 ) ;
#12626 = CARTESIAN_POINT ( 'NONE',  ( 0.000000000000000000, 0.000000000000000000, -0.8000000000000000444 ) ) ;
#12627 = CARTESIAN_POINT ( 'NONE',  ( 19.40000000000002700, 62.98000740192551206, 3.387500001229033941 ) ) ;
#12628 = VERTEX_POINT ( 'NONE', #234 ) ;
#12629 = FILL_AREA_STYLE ('',( #11508 ) ) ;
#12630 = ORIENTED_EDGE ( 'NONE', *, *, #10987, .T. ) ;
#12631 = SURFACE_STYLE_FILL_AREA ( #4522 ) ;
#12632 = EDGE_LOOP ( 'NONE', ( #12742, #7382, #4060, #8829 ) ) ;
#12633 = EDGE_CURVE ( 'NONE', #2177, #11634, #4036, .T. ) ;
#12634 = CARTESIAN_POINT ( 'NONE',  ( 27.76326592528804582, 59.46858721371755507, 3.000000000000000000 ) ) ;
#12635 = DIRECTION ( 'NONE',  ( 0.000000000000000000, 0.000000000000000000, 1.000000000000000000 ) ) ;
#12636 = CIRCLE ( 'NONE', #4695, 3.349999999999995204 ) ;
#12637 = UNCERTAINTY_MEASURE_WITH_UNIT (LENGTH_MEASURE( 1.000000000000000082E-05 ), #2073, 'distance_accuracy_value', 'NONE');
#12638 = CIRCLE ( 'NONE', #8037, 29.99999999999999645 ) ;
#12639 = ORIENTED_EDGE ( 'NONE', *, *, #1888, .F. ) ;
#12640 = CARTESIAN_POINT ( 'NONE',  ( 66.19999999999998863, 90.00000000000000000, 4.774999999999999467 ) ) ;
#12641 = VERTEX_POINT ( 'NONE', #9142 ) ;
#12642 = EDGE_CURVE ( 'NONE', #4450, #11781, #10777, .T. ) ;
#12643 = EDGE_CURVE ( 'NONE', #2484, #7067, #365, .T. ) ;
#12644 = ORIENTED_EDGE ( 'NONE', *, *, #6492, .F. ) ;
#12645 = VECTOR ( 'NONE', #4708, 1000.000000000000000 ) ;
#12646 = CARTESIAN_POINT ( 'NONE',  ( 3.556430356250014579, 108.1539533981018053, 3.471875000614516704 ) ) ;
#12647 = ORIENTED_EDGE ( 'NONE', *, *, #9434, .T. ) ;
#12648 = VECTOR ( 'NONE', #920, 1000.000000000000000 ) ;
#12649 = CARTESIAN_POINT ( 'NONE',  ( 50.59999999999999432, 117.0199925980744666, 3.950000000000000178 ) ) ;
#12650 = CARTESIAN_POINT ( 'NONE',  ( 34.25000000000000000, 93.26496554346289258, 4.000000000000000000 ) ) ;
#12651 = DIRECTION ( 'NONE',  ( -0.000000000000000000, 1.000000000000000000, -0.000000000000000000 ) ) ;
#12652 = CARTESIAN_POINT ( 'NONE',  ( 66.44356964374998142, 108.1539533981018053, 3.265625000614516882 ) ) ;
#12653 = AXIS2_PLACEMENT_3D ( 'NONE', #682, #5465, #5665 ) ;
#12654 = DIRECTION ( 'NONE',  ( -1.000000000000000000, 0.000000000000000000, 0.000000000000000000 ) ) ;
#12655 = AXIS2_PLACEMENT_3D ( 'NONE', #7060, #11043, #12097 ) ;
#12656 = DIRECTION ( 'NONE',  ( 0.8090169943749476733, 0.5877852522924726930, 0.000000000000000000 ) ) ;
#12657 = LINE ( 'NONE', #4611, #10845 ) ;
#12658 = DIRECTION ( 'NONE',  ( -8.673617379884034486E-16, 0.000000000000000000, -1.000000000000000000 ) ) ;
#12659 = DIRECTION ( 'NONE',  ( 0.000000000000000000, 0.000000000000000000, 1.000000000000000000 ) ) ;
#12660 = DIRECTION ( 'NONE',  ( 0.8660254037844400399, 0.000000000000000000, -0.4999999999999975575 ) ) ;
#12661 = CIRCLE ( 'NONE', #8690, 1.599999999999990319 ) ;
#12662 = CARTESIAN_POINT ( 'NONE',  ( 3.556430356250028790, 71.84604660189818048, 3.996875000614517059 ) ) ;
#12663 = ADVANCED_FACE ( 'NONE', ( #5153 ), #3340, .F. ) ;
#12664 = ORIENTED_EDGE ( 'NONE', *, *, #12833, .F. ) ;
#12665 = AXIS2_PLACEMENT_3D ( 'NONE', #704, #11703, #2751 ) ;
#12666 = CARTESIAN_POINT ( 'NONE',  ( 25.00000000000000355, 0.000000000000000000, 7.250000000000000888 ) ) ;
#12667 = EDGE_LOOP ( 'NONE', ( #5672, #2566, #3071, #4955, #7924, #7729, #844, #10119 ) ) ;
#12668 = CARTESIAN_POINT ( 'NONE',  ( -48.33333333333332860, -5.000000000000000000, -1.734723475976807094E-15 ) ) ;
#12669 = DIRECTION ( 'NONE',  ( 0.000000000000000000, -1.000000000000000000, 0.000000000000000000 ) ) ;
#12670 = VECTOR ( 'NONE', #3862, 1000.000000000000000 ) ;
#12671 = ADVANCED_FACE ( 'NONE', ( #12160 ), #6327, .T. ) ;
#12672 = CARTESIAN_POINT ( 'NONE',  ( 17.66025403784438197, 77.14656965084323303, -1.000000000000000000 ) ) ;
#12673 = CARTESIAN_POINT ( 'NONE',  ( 1.040000000000000036, -0.5773502691896256200, -1.000000000000000000 ) ) ;
#12674 = CARTESIAN_POINT ( 'NONE',  ( 51.64126381929429499, 66.24461453698036451, 4.000000000000000000 ) ) ;
#12675 = CARTESIAN_POINT ( 'NONE',  ( 48.49999999999995737, 86.00000000000000000, -10.00000000000000000 ) ) ;
#12676 = EDGE_CURVE ( 'NONE', #1939, #8099, #11365, .T. ) ;
#12677 = ORIENTED_EDGE ( 'NONE', *, *, #10679, .T. ) ;
#12678 = FACE_OUTER_BOUND ( 'NONE', #5329, .T. ) ;
#12679 = EDGE_LOOP ( 'NONE', ( #1114, #7969, #6216, #8005 ) ) ;
#12680 = AXIS2_PLACEMENT_3D ( 'NONE', #8930, #1809, #943 ) ;
#12681 = CARTESIAN_POINT ( 'NONE',  ( 50.60000000000001563, 62.98000740192552627, 3.912500001229034297 ) ) ;
#12682 = DIRECTION ( 'NONE',  ( -1.000000000000000000, 0.000000000000000000, 0.000000000000000000 ) ) ;
#12683 = DIRECTION ( 'NONE',  ( 0.000000000000000000, 0.000000000000000000, 1.000000000000000000 ) ) ;
#12684 = DIRECTION ( 'NONE',  ( 1.000000000000000000, 0.000000000000000000, -0.000000000000000000 ) ) ;
#12685 = FACE_BOUND ( 'NONE', #423, .T. ) ;
#12686 = ORIENTED_EDGE ( 'NONE', *, *, #5837, .F. ) ;
#12687 = LINE ( 'NONE', #11637, #8045 ) ;
#12688 = CONTEXT_DEPENDENT_SHAPE_REPRESENTATION ( #6086, #10758 ) ;
#12689 = CARTESIAN_POINT ( 'NONE',  ( 21.49999999999998579, 94.00000000000000000, -8.000000000000000000 ) ) ;
#12690 = ADVANCED_FACE ( 'NONE', ( #11171 ), #11237, .T. ) ;
#12691 = AXIS2_PLACEMENT_3D ( 'NONE', #10174, #6248, #8350 ) ;
#12692 = ORIENTED_EDGE ( 'NONE', *, *, #6306, .T. ) ;
#12693 = CARTESIAN_POINT ( 'NONE',  ( -28.99038105676692112, 50.21281292110204930, 1.000000000000000000 ) ) ;
#12694 = ORIENTED_EDGE ( 'NONE', *, *, #4843, .T. ) ;
#12695 = FACE_OUTER_BOUND ( 'NONE', #6915, .T. ) ;
#12696 = EDGE_LOOP ( 'NONE', ( #8798, #6968, #11050, #11948 ) ) ;
#12697 = CARTESIAN_POINT ( 'NONE',  ( -60.00000000000000000, -6.000000000000000000, -15.00000000000000355 ) ) ;
#12698 = DIRECTION ( 'NONE',  ( -0.000000000000000000, -0.000000000000000000, -1.000000000000000000 ) ) ;
#12699 = CIRCLE ( 'NONE', #4136, 3.500000000000003109 ) ;
#12700 = EDGE_LOOP ( 'NONE', ( #5670, #6820, #9749, #12448 ) ) ;
#12701 = CARTESIAN_POINT ( 'NONE',  ( -57.99999999999999289, 30.00000000000000000, 9.999999999999996447 ) ) ;
#12702 = ORIENTED_EDGE ( 'NONE', *, *, #10688, .F. ) ;
#12703 = DIRECTION ( 'NONE',  ( -0.000000000000000000, -0.000000000000000000, -1.000000000000000000 ) ) ;
#12704 = EDGE_CURVE ( 'NONE', #8351, #4553, #4249, .T. ) ;
#12705 = EDGE_LOOP ( 'NONE', ( #8428, #3742, #3231, #6777 ) ) ;
#12706 = CARTESIAN_POINT ( 'NONE',  ( 66.44356964374999563, 90.00000000000000000, 4.128125000614517148 ) ) ;
#12707 = VERTEX_POINT ( 'NONE', #8369 ) ;
#12708 = VECTOR ( 'NONE', #8320, 1000.000000000000000 ) ;
#12709 = DIRECTION ( 'NONE',  ( -0.000000000000000000, -0.000000000000000000, -1.000000000000000000 ) ) ;
#12710 = LINE ( 'NONE', #3813, #2878 ) ;
#12711 = CARTESIAN_POINT ( 'NONE',  ( 66.44356964374999563, 90.00000000000000000, 3.678125000614516971 ) ) ;
#12712 = EDGE_CURVE ( 'NONE', #7376, #10818, #61, .T. ) ;
#12713 = ADVANCED_FACE ( 'NONE', ( #6128, #12225 ), #1228, .T. ) ;
#12714 = FACE_OUTER_BOUND ( 'NONE', #9304, .T. ) ;
#12715 = VECTOR ( 'NONE', #285, 1000.000000000000000 ) ;
#12716 = AXIS2_PLACEMENT_3D ( 'NONE', #2229, #12093, #8237 ) ;
#12717 = DIRECTION ( 'NONE',  ( -0.000000000000000000, 1.000000000000000000, -0.000000000000000000 ) ) ;
#12718 = CARTESIAN_POINT ( 'NONE',  ( 4.999999999999962697, 79.07477288111861924, 3.000000000000000000 ) ) ;
#12719 = CARTESIAN_POINT ( 'NONE',  ( 24.44860983802972498, 119.5968892347202654, 2.999999999999997780 ) ) ;
#12720 = ADVANCED_FACE ( 'NONE', ( #11103 ), #9276, .T. ) ;
#12721 = CARTESIAN_POINT ( 'NONE',  ( 35.00000000000000000, 90.00000000000000000, 4.000000000000000000 ) ) ;
#12722 = CARTESIAN_POINT ( 'NONE',  ( 45.00000000000000000, 2.000000000000000000, 7.349999999999994316 ) ) ;
#12723 = CARTESIAN_POINT ( 'NONE',  ( 19.27821517812500574, 117.2309300971526937, 2.984375000614517326 ) ) ;
#12724 = ORIENTED_EDGE ( 'NONE', *, *, #11466, .T. ) ;
#12725 = VECTOR ( 'NONE', #8401, 1000.000000000000000 ) ;
#12726 = CARTESIAN_POINT ( 'NONE',  ( 3.800000000000015365, 108.0133283987163111, 3.612500000000000711 ) ) ;
#12727 = DIRECTION ( 'NONE',  ( -0.000000000000000000, -0.000000000000000000, 1.000000000000000000 ) ) ;
#12728 = ORIENTED_EDGE ( 'NONE', *, *, #4873, .T. ) ;
#12729 = FILL_AREA_STYLE_COLOUR ( '', #2589 ) ;
#12730 = EDGE_CURVE ( 'NONE', #4783, #11942, #166, .T. ) ;
#12731 = VECTOR ( 'NONE', #637, 1000.000000000000000 ) ;
#12732 = CARTESIAN_POINT ( 'NONE',  ( 3.033375984251971413, -3.035766082959412415E-15, 0.000000000000000000 ) ) ;
#12733 = FACE_OUTER_BOUND ( 'NONE', #9081, .T. ) ;
#12734 = VECTOR ( 'NONE', #5515, 1000.000000000000114 ) ;
#12735 = DIRECTION ( 'NONE',  ( -0.000000000000000000, -0.000000000000000000, -1.000000000000000000 ) ) ;
#12736 = CARTESIAN_POINT ( 'NONE',  ( 3.556430356250028790, 71.84604660189818048, 4.390625000614517326 ) ) ;
#12737 = DIRECTION ( 'NONE',  ( -0.8660254037844360431, -0.5000000000000047740, -0.000000000000000000 ) ) ;
#12738 = CARTESIAN_POINT ( 'NONE',  ( 66.44356964375000985, 71.84604660189820891, 4.146875000614517859 ) ) ;
#12739 = ORIENTED_EDGE ( 'NONE', *, *, #7265, .F. ) ;
#12740 = VECTOR ( 'NONE', #4400, 1000.000000000000114 ) ;
#12741 = CARTESIAN_POINT ( 'NONE',  ( 62.42613047537196991, 99.43702109502110886, 0.6666666666666665186 ) ) ;
#12742 = ORIENTED_EDGE ( 'NONE', *, *, #9631, .T. ) ;
#12743 = DIRECTION ( 'NONE',  ( 0.000000000000000000, 0.000000000000000000, -1.000000000000000000 ) ) ;
#12744 = DIRECTION ( 'NONE',  ( -1.000000000000000000, -0.000000000000000000, -0.000000000000000000 ) ) ;
#12745 = CARTESIAN_POINT ( 'NONE',  ( -16.33333333333332504, 46.12451549659709116, 7.999999999999996447 ) ) ;
#12746 = ADVANCED_FACE ( 'NONE', ( #10646 ), #1748, .F. ) ;
#12747 = DIRECTION ( 'NONE',  ( 0.000000000000000000, 0.000000000000000000, 1.000000000000000000 ) ) ;
#12749 = DIRECTION ( 'NONE',  ( -0.000000000000000000, -0.000000000000000000, -1.000000000000000000 ) ) ;
#12748 = AXIS2_PLACEMENT_3D ( 'NONE', #8166, #4178, #11163 ) ;
#12750 = EDGE_LOOP ( 'NONE', ( #7960, #11457, #5899, #26 ) ) ;
#12751 = LINE ( 'NONE', #6788, #3456 ) ;
#12752 = PLANE ( 'NONE',  #12952 ) ;
#12753 = ORIENTED_EDGE ( 'NONE', *, *, #6043, .T. ) ;
#12754 = DIRECTION ( 'NONE',  ( -0.000000000000000000, -1.000000000000000000, -0.000000000000000000 ) ) ;
#12755 = ORIENTED_EDGE ( 'NONE', *, *, #3830, .F. ) ;
#12756 = ORIENTED_EDGE ( 'NONE', *, *, #11382, .F. ) ;
#12757 = CARTESIAN_POINT ( 'NONE',  ( 25.00000000000000355, -5.000000000000000000, 7.250000000000000888 ) ) ;
#12758 = VECTOR ( 'NONE', #10041, 1000.000000000000000 ) ;
#12759 = CARTESIAN_POINT ( 'NONE',  ( -62.98205080756885366, 29.16506350946109194, 0.000000000000000000 ) ) ;
#12760 = CIRCLE ( 'NONE', #7508, 3.500000000000003109 ) ;
#12761 = EDGE_CURVE ( 'NONE', #1154, #6795, #2482, .T. ) ;
#12762 = EDGE_CURVE ( 'NONE', #9386, #9145, #7156, .T. ) ;
#12763 = ORIENTED_EDGE ( 'NONE', *, *, #6720, .F. ) ;
#12764 = DIRECTION ( 'NONE',  ( 0.000000000000000000, 0.000000000000000000, -1.000000000000000000 ) ) ;
#12765 = VERTEX_POINT ( 'NONE', #691 ) ;
#12766 = FACE_BOUND ( 'NONE', #11902, .T. ) ;
#12767 = ORIENTED_EDGE ( 'NONE', *, *, #3724, .F. ) ;
#12768 = AXIS2_PLACEMENT_3D ( 'NONE', #10224, #10157, #5441 ) ;
#12769 = CARTESIAN_POINT ( 'NONE',  ( 66.44356964374999563, 71.84604660189820891, 3.640625000614517326 ) ) ;
#12770 = ORIENTED_EDGE ( 'NONE', *, *, #9603, .F. ) ;
#12771 = CARTESIAN_POINT ( 'NONE',  ( 13.53859087060910404, 112.9805567844265539, 2.999999999999999112 ) ) ;
#12772 = LINE ( 'NONE', #12832, #6618 ) ;
#12773 = DIRECTION ( 'NONE',  ( -0.3262398754384822630, 0.9452870165584014162, 0.000000000000000000 ) ) ;
#12774 = CARTESIAN_POINT ( 'NONE',  ( 50.72178482187501203, 62.76906990284730625, 3.603125000614517681 ) ) ;
#12775 = EDGE_CURVE ( 'NONE', #10536, #8908, #1087, .T. ) ;
#12776 = CIRCLE ( 'NONE', #3381, 1.599999999999986766 ) ;
#12777 = FACE_OUTER_BOUND ( 'NONE', #4084, .T. ) ;
#12778 = CARTESIAN_POINT ( 'NONE',  ( 35.00000000000000000, 90.00000000000000000, 6.000000000000000000 ) ) ;
#12779 = FACE_BOUND ( 'NONE', #8200, .T. ) ;
#12780 = PLANE ( 'NONE',  #2511 ) ;
#12781 = DIRECTION ( 'NONE',  ( -1.000000000000000000, 0.000000000000000000, 0.000000000000000000 ) ) ;
#12782 = DIRECTION ( 'NONE',  ( -5.624500927088228034E-17, 1.370729058197317775E-18, 1.000000000000000000 ) ) ;
#12783 = AXIS2_PLACEMENT_3D ( 'NONE', #11099, #2527, #4551 ) ;
#12784 =( REPRESENTATION_RELATIONSHIP ('NONE','NONE', #1997, #9523 ) REPRESENTATION_RELATIONSHIP_WITH_TRANSFORMATION ( #3858 )SHAPE_REPRESENTATION_RELATIONSHIP( ) );
#12785 = CARTESIAN_POINT ( 'NONE',  ( 3.556430356250028790, 71.84604660189818048, 4.446875000614517681 ) ) ;
#12786 = EDGE_LOOP ( 'NONE', ( #8650, #2144, #2009, #2345 ) ) ;
#12787 = CARTESIAN_POINT ( 'NONE',  ( 66.19999999999997442, 108.0133283987163253, 4.362499999999999822 ) ) ;
#12788 = CARTESIAN_POINT ( 'NONE',  ( 35.00000000000000000, 126.0266567974326222, 3.650000001229033675 ) ) ;
#12789 = VERTEX_POINT ( 'NONE', #8688 ) ;
#12790 = AXIS2_PLACEMENT_3D ( 'NONE', #12369, #11253, #3223 ) ;
#12791 = DIRECTION ( 'NONE',  ( 1.000000000000000000, 0.000000000000000000, 0.000000000000000000 ) ) ;
#12792 = DIRECTION ( 'NONE',  ( 0.000000000000000000, 0.000000000000000000, 1.000000000000000000 ) ) ;
#12793 = CYLINDRICAL_SURFACE ( 'NONE', #12454, 1.500000000000001332 ) ;
#12794 = EDGE_CURVE ( 'NONE', #11762, #5032, #496, .T. ) ;
#12795 = CARTESIAN_POINT ( 'NONE',  ( 66.44356964375000985, 71.84604660189820891, 3.640625000614517326 ) ) ;
#12796 = EDGE_CURVE ( 'NONE', #7089, #451, #11275, .T. ) ;
#12797 = CARTESIAN_POINT ( 'NONE',  ( 8.500000000000000000, 66.25713400046146262, -1.000000000000000666 ) ) ;
#12798 = DIRECTION ( 'NONE',  ( -0.000000000000000000, 1.000000000000000000, -0.000000000000000000 ) ) ;
#12799 = VERTEX_POINT ( 'NONE', #564 ) ;
#12800 = LINE ( 'NONE', #3843, #9340 ) ;
#12801 = ORIENTED_EDGE ( 'NONE', *, *, #5274, .T. ) ;
#12802 = LINE ( 'NONE', #9793, #589 ) ;
#12803 = CARTESIAN_POINT ( 'NONE',  ( 25.00000000000000355, 0.000000000000000000, 5.750000000000000000 ) ) ;
#12804 = DIRECTION ( 'NONE',  ( -1.000000000000000000, 0.000000000000000000, 0.000000000000000000 ) ) ;
#12805 = DIRECTION ( 'NONE',  ( 1.000000000000000000, 0.000000000000000000, 0.000000000000000000 ) ) ;
#12806 = FACE_OUTER_BOUND ( 'NONE', #11423, .T. ) ;
#12807 = ORIENTED_EDGE ( 'NONE', *, *, #10102, .F. ) ;
#12808 = CARTESIAN_POINT ( 'NONE',  ( -61.13397459621560159, 31.96410161513775350, 0.000000000000000000 ) ) ;
#12809 = CARTESIAN_POINT ( 'NONE',  ( 0.000000000000000000, 0.4117131682837005258, -0.8000000000000000444 ) ) ;
#12810 = ORIENTED_EDGE ( 'NONE', *, *, #3712, .T. ) ;
#12811 = VECTOR ( 'NONE', #4828, 1000.000000000000000 ) ;
#12812 = FACE_OUTER_BOUND ( 'NONE', #4434, .T. ) ;
#12813 = ORIENTED_EDGE ( 'NONE', *, *, #11638, .T. ) ;
#12814 = CYLINDRICAL_SURFACE ( 'NONE', #5261, 28.99999999999999289 ) ;
#12815 = VERTEX_POINT ( 'NONE', #4571 ) ;
#12816 = ADVANCED_FACE ( 'NONE', ( #2675 ), #11689, .T. ) ;
#12817 = DIRECTION ( 'NONE',  ( 1.000000000000000000, 0.000000000000000000, 0.000000000000000000 ) ) ;
#12818 = MECHANICAL_DESIGN_GEOMETRIC_PRESENTATION_REPRESENTATION (  '', ( #12194 ), #5299 ) ;
#12819 = CARTESIAN_POINT ( 'NONE',  ( -0.2000000000000000111, -6.446898479113814417, -0.8000000000000000444 ) ) ;
#12820 = VECTOR ( 'NONE', #5925, 1000.000000000000000 ) ;
#12821 = VERTEX_POINT ( 'NONE', #5735 ) ;
#12822 = DIRECTION ( 'NONE',  ( 1.000000000000000000, 0.000000000000000000, 0.000000000000000000 ) ) ;
#12823 = ORIENTED_EDGE ( 'NONE', *, *, #5879, .T. ) ;
#12824 = DIRECTION ( 'NONE',  ( 0.000000000000000000, 0.000000000000000000, 1.000000000000000000 ) ) ;
#12825 =( GEOMETRIC_REPRESENTATION_CONTEXT ( 3 ) GLOBAL_UNCERTAINTY_ASSIGNED_CONTEXT ( ( #2121 ) ) GLOBAL_UNIT_ASSIGNED_CONTEXT ( ( #3271, #10449, #12550 ) ) REPRESENTATION_CONTEXT ( 'NONE', 'WORKASPACE' ) );
#12826 = ORIENTED_EDGE ( 'NONE', *, *, #5002, .T. ) ;
#12827 = ADVANCED_FACE ( 'NONE', ( #2740 ), #9871, .F. ) ;
#12828 = CARTESIAN_POINT ( 'NONE',  ( 66.44356964374998142, 108.1539533981018053, 4.615625000614516971 ) ) ;
#12829 = ORIENTED_EDGE ( 'NONE', *, *, #12602, .F. ) ;
#12830 = CARTESIAN_POINT ( 'NONE',  ( 1.749999999999999112, 0.000000000000000000, 1.599999999999998757 ) ) ;
#12831 = AXIS2_PLACEMENT_3D ( 'NONE', #2980, #6964, #10949 ) ;
#12832 = CARTESIAN_POINT ( 'NONE',  ( -60.00000000000000000, 30.00000000000000000, -10.00000000000000355 ) ) ;
#12833 = EDGE_CURVE ( 'NONE', #9167, #4318, #12416, .T. ) ;
#12834 = VECTOR ( 'NONE', #4622, 1000.000000000000000 ) ;
#12835 = DIRECTION ( 'NONE',  ( -1.000000000000000000, 0.000000000000000000, 0.000000000000000000 ) ) ;
#12836 = CARTESIAN_POINT ( 'NONE',  ( 50.72178482187501203, 62.76906990284730625, 3.153125000614517504 ) ) ;
#12837 = DIRECTION ( 'NONE',  ( 0.000000000000000000, 0.000000000000000000, -1.000000000000000000 ) ) ;
#12838 = CARTESIAN_POINT ( 'NONE',  ( -48.33333333333332860, -5.000000000000000000, -1.734723475976807094E-15 ) ) ;
#12839 = VERTEX_POINT ( 'NONE', #5673 ) ;
#12840 = CIRCLE ( 'NONE', #1558, 3.350000000000000089 ) ;
#12841 = CARTESIAN_POINT ( 'NONE',  ( 65.00000000000000000, 90.00000000000000000, -3.000000000000000000 ) ) ;
#12842 = CARTESIAN_POINT ( 'NONE',  ( 13.95244456248789788, 109.9499476216067819, 4.000000000000000000 ) ) ;
#12843 = ORIENTED_EDGE ( 'NONE', *, *, #7949, .T. ) ;
#12844 = CIRCLE ( 'NONE', #7417, 3.500000000000003109 ) ;
#12845 =( BOUNDED_CURVE ( )  B_SPLINE_CURVE ( 2, ( #5193, #206, #8660, #2714, #5448, #7677, #11665 ),
 .UNSPECIFIED., .F., .F. ) 
 B_SPLINE_CURVE_WITH_KNOTS ( ( 3, 2, 2, 3 ),
 ( 0.3000000000000002109, 0.3333333333333334259, 0.3666666666666666963, 0.3999999999999999667 ),
 .UNSPECIFIED. ) 
 CURVE ( )  GEOMETRIC_REPRESENTATION_ITEM ( )  RATIONAL_B_SPLINE_CURVE ( ( 0.9999999999999991118, 0.8660254037844395958, 1.000000000000000000, 0.8660254037844387076, 1.000000000000000000, 0.8660254037844389297, 0.9999999999999997780 ) ) 
 REPRESENTATION_ITEM ( '' )  );
#12846 = DIRECTION ( 'NONE',  ( -1.000000000000000000, 0.000000000000000000, 0.000000000000000000 ) ) ;
#12847 = EDGE_LOOP ( 'NONE', ( #4600, #557, #1335, #1981 ) ) ;
#12848 = EDGE_CURVE ( 'NONE', #11167, #3079, #8500, .T. ) ;
#12849 = DIRECTION ( 'NONE',  ( 1.000000000000000000, 0.000000000000000000, 0.000000000000000000 ) ) ;
#12850 = CARTESIAN_POINT ( 'NONE',  ( 66.44356964374999563, 90.00000000000000000, 3.734375000614516882 ) ) ;
#12851 = VERTEX_POINT ( 'NONE', #3467 ) ;
#12852 = CARTESIAN_POINT ( 'NONE',  ( 35.00000000000000711, 53.97334320256736362, 3.312500000000000000 ) ) ;
#12853 = DIRECTION ( 'NONE',  ( 1.000000000000000000, 0.000000000000000000, 0.000000000000000000 ) ) ;
#12854 = ORIENTED_EDGE ( 'NONE', *, *, #6371, .T. ) ;
#12855 = AXIS2_PLACEMENT_3D ( 'NONE', #9396, #2409, #10250 ) ;
#12856 = AXIS2_PLACEMENT_3D ( 'NONE', #6592, #2487, #10460 ) ;
#12857 = CARTESIAN_POINT ( 'NONE',  ( 1.000000000000000000, -4.273461295629625845, -0.8000000000000000444 ) ) ;
#12858 = DIRECTION ( 'NONE',  ( -1.000000000000000000, -0.000000000000000000, -0.000000000000000000 ) ) ;
#12859 = CIRCLE ( 'NONE', #1580, 1.500000000000001332 ) ;
#12860 = CARTESIAN_POINT ( 'NONE',  ( 64.39470308771993246, 100.6987976320522336, 2.952601389814389687 ) ) ;
#12861 = EDGE_CURVE ( 'NONE', #6204, #10216, #3529, .T. ) ;
#12862 = CIRCLE ( 'NONE', #12242, 0.5999999999999998668 ) ;
#12863 = CARTESIAN_POINT ( 'NONE',  ( 35.75000000000000711, 93.41869858279433458, 6.000000000000000000 ) ) ;
#12864 = CARTESIAN_POINT ( 'NONE',  ( 66.44356964374999563, 90.00000000000000000, 4.184375000614516615 ) ) ;
#12865 = ORIENTED_EDGE ( 'NONE', *, *, #11705, .F. ) ;
#12866 = CARTESIAN_POINT ( 'NONE',  ( -60.00000000000000000, 30.00000000000000000, 3.000000000000000000 ) ) ;
#12867 = ORIENTED_EDGE ( 'NONE', *, *, #8400, .F. ) ;
#12868 = CIRCLE ( 'NONE', #4311, 3.500000000000003109 ) ;
#12869 = EDGE_CURVE ( 'NONE', #12039, #8524, #3594, .T. ) ;
#12870 = EDGE_CURVE ( 'NONE', #571, #7840, #1490, .T. ) ;
#12871 = MECHANICAL_DESIGN_GEOMETRIC_PRESENTATION_REPRESENTATION (  '', ( #2860 ), #324 ) ;
#12872 = PRODUCT_DEFINITION_CONTEXT ( 'detailed design', #2267, 'design' ) ;
#12873 = CARTESIAN_POINT ( 'NONE',  ( 19.40000000000000924, 117.0199925980744666, 3.575000000000000178 ) ) ;
#12874 = CARTESIAN_POINT ( 'NONE',  ( 72.83557806687970526, 62.54593364529978317, -0.9999999999999970024 ) ) ;
#12875 = CARTESIAN_POINT ( 'NONE',  ( -54.07179676972453564, 35.73205080756890339, 1.000000000000000000 ) ) ;
#12876 = LINE ( 'NONE', #9735, #4792 ) ;
#12877 = ORIENTED_EDGE ( 'NONE', *, *, #1839, .F. ) ;
#12878 = DIRECTION ( 'NONE',  ( -0.8660254037844360431, -0.5000000000000047740, -0.000000000000000000 ) ) ;
#12879 = CONTEXT_DEPENDENT_SHAPE_REPRESENTATION ( #5422, #1778 ) ;
#12880 = DIRECTION ( 'NONE',  ( -0.000000000000000000, -0.000000000000000000, -1.000000000000000000 ) ) ;
#12881 = ORIENTED_EDGE ( 'NONE', *, *, #7105, .F. ) ;
#12882 = EDGE_CURVE ( 'NONE', #10133, #4212, #5475, .T. ) ;
#12883 = CARTESIAN_POINT ( 'NONE',  ( 0.000000000000000000, 0.000000000000000000, -0.8000000000000000444 ) ) ;
#12884 = ORIENTED_EDGE ( 'NONE', *, *, #12794, .T. ) ;
#12885 = VECTOR ( 'NONE', #2864, 1000.000000000000000 ) ;
#12886 = DIRECTION ( 'NONE',  ( 1.000000000000000000, 0.000000000000000000, -1.445602896647339656E-17 ) ) ;
#12887 = ORIENTED_EDGE ( 'NONE', *, *, #10862, .F. ) ;
#12888 = DIRECTION ( 'NONE',  ( -5.624500927088228034E-17, 1.370729058197317775E-18, 1.000000000000000000 ) ) ;
#12889 = CYLINDRICAL_SURFACE ( 'NONE', #9988, 3.350000000000003642 ) ;
#12890 = ORIENTED_EDGE ( 'NONE', *, *, #4794, .F. ) ;
#12891 = DIRECTION ( 'NONE',  ( 0.000000000000000000, 1.000000000000000000, 0.000000000000000000 ) ) ;
#12892 = VERTEX_POINT ( 'NONE', #10518 ) ;
#12893 = ADVANCED_FACE ( 'NONE', ( #2610 ), #1623, .T. ) ;
#12894 = CARTESIAN_POINT ( 'NONE',  ( -63.99999999999998579, 36.92820323027551410, 2.500000000000000000 ) ) ;
#12895 = ORIENTED_EDGE ( 'NONE', *, *, #4844, .F. ) ;
#12896 = CARTESIAN_POINT ( 'NONE',  ( 3.556430356250015024, 90.00000000000000000, 3.453125000614517770 ) ) ;
#12897 = ORIENTED_EDGE ( 'NONE', *, *, #5464, .T. ) ;
#12898 = DIRECTION ( 'NONE',  ( 0.000000000000000000, 0.000000000000000000, 1.000000000000000000 ) ) ;
#12899 = CARTESIAN_POINT ( 'NONE',  ( 19.40000000000000924, 117.0199925980744666, 4.025000000000000355 ) ) ;
#12900 = VECTOR ( 'NONE', #6634, 1000.000000000000000 ) ;
#12901 = CARTESIAN_POINT ( 'NONE',  ( 3.800000000000015810, 108.0133283987162969, 4.962499999999999467 ) ) ;
#12902 = CARTESIAN_POINT ( 'NONE',  ( 64.54728994471078352, 100.7543353520590870, 2.802601390178781404 ) ) ;
#12903 = FACE_OUTER_BOUND ( 'NONE', #8300, .T. ) ;
#12904 = ORIENTED_EDGE ( 'NONE', *, *, #3963, .T. ) ;
#12905 = FACE_BOUND ( 'NONE', #9231, .T. ) ;
#12906 = EDGE_CURVE ( 'NONE', #6452, #9676, #12601, .T. ) ;
#12907 = DIRECTION ( 'NONE',  ( 0.000000000000000000, 0.000000000000000000, 1.000000000000000000 ) ) ;
#12908 = CARTESIAN_POINT ( 'NONE',  ( 16.01593418524656798, 115.0585008649344019, 3.000000000000000888 ) ) ;
#12909 = AXIS2_PLACEMENT_3D ( 'NONE', #7270, #6085, #6020 ) ;
#12910 = VERTEX_POINT ( 'NONE', #11022 ) ;
#12911 = CARTESIAN_POINT ( 'NONE',  ( 7.369500000000001272, 1.836970198721029934E-16, -1.500000000000000000 ) ) ;
#12912 = ORIENTED_EDGE ( 'NONE', *, *, #3799, .T. ) ;
#12913 = CARTESIAN_POINT ( 'NONE',  ( 33.50000000000000711, 79.80000000000001137, 6.000000000000000000 ) ) ;
#12914 = CARTESIAN_POINT ( 'NONE',  ( 66.44356964374999563, 90.00000000000000000, 4.184375000614516615 ) ) ;
#12915 = VERTEX_POINT ( 'NONE', #4949 ) ;
#12916 = CARTESIAN_POINT ( 'NONE',  ( 3.556430356250014579, 108.1539533981018053, 3.471875000614516704 ) ) ;
#12917 = CARTESIAN_POINT ( 'NONE',  ( 3.800000000000015365, 90.00000000000000000, 3.200000000000000178 ) ) ;
#12918 = AXIS2_PLACEMENT_3D ( 'NONE', #1750, #321, #7578 ) ;
#12919 = VECTOR ( 'NONE', #10911, 1000.000000000000114 ) ;
#12920 = EDGE_CURVE ( 'NONE', #9660, #11844, #8026, .T. ) ;
#12921 = DIRECTION ( 'NONE',  ( -0.000000000000000000, -0.000000000000000000, -1.000000000000000000 ) ) ;
#12922 = ADVANCED_FACE ( 'NONE', ( #12011 ), #820, .T. ) ;
#12923 = PLANE ( 'NONE',  #8457 ) ;
#12924 = CARTESIAN_POINT ( 'NONE',  ( -60.00000000000000000, 23.99999999999998934, -2.500000000000000000 ) ) ;
#12925 = AXIS2_PLACEMENT_3D ( 'NONE', #4540, #11465, #2452 ) ;
#12926 = CARTESIAN_POINT ( 'NONE',  ( 9.650000000000000355, 0.000000000000000000, 1.219500000000000028 ) ) ;
#12927 = CARTESIAN_POINT ( 'NONE',  ( -6.666666666666660745, 2.000000000000001332, 0.000000000000000000 ) ) ;
#12928 = ORIENTED_EDGE ( 'NONE', *, *, #1486, .F. ) ;
#12929 = LINE ( 'NONE', #10956, #11842 ) ;
#12930 = VERTEX_POINT ( 'NONE', #7828 ) ;
#12931 = DIRECTION ( 'NONE',  ( 1.000000000000000000, 0.000000000000000000, 4.336808689942017243E-16 ) ) ;
#12932 = EDGE_CURVE ( 'NONE', #41, #3514, #10836, .T. ) ;
#12933 = CIRCLE ( 'NONE', #9376, 30.19999999999999218 ) ;
#12934 = DIRECTION ( 'NONE',  ( 1.000000000000000000, 0.000000000000000000, 0.000000000000000000 ) ) ;
#12935 = CARTESIAN_POINT ( 'NONE',  ( 64.31840955652153013, 100.6710290542226431, 2.929163888449521025 ) ) ;
#12936 = LINE ( 'NONE', #8753, #5507 ) ;
#12937 = ORIENTED_EDGE ( 'NONE', *, *, #1279, .F. ) ;
#12938 = ADVANCED_BREP_SHAPE_REPRESENTATION ( '', ( #12156, #5704 ), #1107 ) ;
#12939 = LINE ( 'NONE', #2082, #9717 ) ;
#12940 = CARTESIAN_POINT ( 'NONE',  ( 35.00000000000000000, 90.00000000000000000, 4.800000000000000711 ) ) ;
#12941 = VERTEX_POINT ( 'NONE', #5920 ) ;
#12942 = CIRCLE ( 'NONE', #5000, 31.19999999999999218 ) ;
#12943 = FILL_AREA_STYLE ('',( #960 ) ) ;
#12944 = DIRECTION ( 'NONE',  ( 0.000000000000000000, 0.000000000000000000, 1.000000000000000000 ) ) ;
#12945 = EDGE_LOOP ( 'NONE', ( #11307, #4066, #9415, #4102 ) ) ;
#12946 = AXIS2_PLACEMENT_3D ( 'NONE', #2453, #6426, #10425 ) ;
#12947 = EDGE_CURVE ( 'NONE', #1634, #10264, #2931, .T. ) ;
#12948 = ORIENTED_EDGE ( 'NONE', *, *, #9639, .T. ) ;
#12949 = CARTESIAN_POINT ( 'NONE',  ( 35.00000000000000000, 90.00000000000000000, -3.799999999999999822 ) ) ;
#12950 = FACE_OUTER_BOUND ( 'NONE', #8638, .T. ) ;
#12951 = ORIENTED_EDGE ( 'NONE', *, *, #2336, .F. ) ;
#12952 = AXIS2_PLACEMENT_3D ( 'NONE', #8697, #958, #2939 ) ;
#12953 = ORIENTED_EDGE ( 'NONE', *, *, #1023, .F. ) ;
#12954 = ORIENTED_EDGE ( 'NONE', *, *, #5063, .T. ) ;
#12955 = NEXT_ASSEMBLY_USAGE_OCCURRENCE ( 'NAUO1', ' ', ' ', #11777, #10725, $ ) ;
#12956 = NEXT_ASSEMBLY_USAGE_OCCURRENCE ( 'NAUO2', ' ', ' ', #11777, #8584, $ ) ;
#12957 = NEXT_ASSEMBLY_USAGE_OCCURRENCE ( 'NAUO3', ' ', ' ', #11777, #5290, $ ) ;
#12958 = NEXT_ASSEMBLY_USAGE_OCCURRENCE ( 'NAUO4', ' ', ' ', #11777, #8014, $ ) ;
#12959 = NEXT_ASSEMBLY_USAGE_OCCURRENCE ( 'NAUO5', ' ', ' ', #11777, #12256, $ ) ;
#12960 = NEXT_ASSEMBLY_USAGE_OCCURRENCE ( 'NAUO6', ' ', ' ', #11777, #10165, $ ) ;
#12961 = NEXT_ASSEMBLY_USAGE_OCCURRENCE ( 'NAUO7', ' ', ' ', #11777, #2349, $ ) ;
#12962 = NEXT_ASSEMBLY_USAGE_OCCURRENCE ( 'NAUO8', ' ', ' ', #11777, #10255, $ ) ;
#12963 = NEXT_ASSEMBLY_USAGE_OCCURRENCE ( 'NAUO9', ' ', ' ', #11777, #12586, $ ) ;
#12964 = NEXT_ASSEMBLY_USAGE_OCCURRENCE ( 'NAUO10', ' ', ' ', #11777, #12586, $ ) ;
#12965 = NEXT_ASSEMBLY_USAGE_OCCURRENCE ( 'NAUO11', ' ', ' ', #11777, #9854, $ ) ;
#12966 = NEXT_ASSEMBLY_USAGE_OCCURRENCE ( 'NAUO12', ' ', ' ', #11777, #9854, $ ) ;
#12967 = NEXT_ASSEMBLY_USAGE_OCCURRENCE ( 'NAUO13', ' ', ' ', #11777, #3872, $ ) ;
#12968 = NEXT_ASSEMBLY_USAGE_OCCURRENCE ( 'NAUO14', ' ', ' ', #11777, #3872, $ ) ;
#12969 = NEXT_ASSEMBLY_USAGE_OCCURRENCE ( 'NAUO15', ' ', ' ', #11777, #3872, $ ) ;
#12970 = NEXT_ASSEMBLY_USAGE_OCCURRENCE ( 'NAUO16', ' ', ' ', #11777, #3872, $ ) ;
#12971 = NEXT_ASSEMBLY_USAGE_OCCURRENCE ( 'NAUO17', ' ', ' ', #11777, #3872, $ ) ;
#12972 = NEXT_ASSEMBLY_USAGE_OCCURRENCE ( 'NAUO18', ' ', ' ', #11777, #3872, $ ) ;
#12973 = NEXT_ASSEMBLY_USAGE_OCCURRENCE ( 'NAUO19', ' ', ' ', #11777, #3872, $ ) ;
#12974 = NEXT_ASSEMBLY_USAGE_OCCURRENCE ( 'NAUO20', ' ', ' ', #11777, #3872, $ ) ;
#12975=COLOUR_RGB('Dark Blue',0.08,0.2,0.34);
#12976=FILL_AREA_STYLE_COLOUR('',#12975);
#12977=FILL_AREA_STYLE('',(#12976));
#12978=SURFACE_STYLE_FILL_AREA(#12977);
#12979=SURFACE_SIDE_STYLE('',(#12978));
#12980=SURFACE_STYLE_USAGE(.BOTH.,#12979);
#12981=PRESENTATION_STYLE_ASSIGNMENT((#12980));
#12982=COLOUR_RGB('Light Blue',0.38,0.62,0.78);
#12983=FILL_AREA_STYLE_COLOUR('',#12982);
#12984=FILL_AREA_STYLE('',(#12983));
#12985=SURFACE_STYLE_FILL_AREA(#12984);
#12986=SURFACE_SIDE_STYLE('',(#12985));
#12987=SURFACE_STYLE_USAGE(.BOTH.,#12986);
#12988=PRESENTATION_STYLE_ASSIGNMENT((#12987));
#12989=COLOUR_RGB('Sky Blue',0.24,0.69,0.87);
#12990=FILL_AREA_STYLE_COLOUR('',#12989);
#12991=FILL_AREA_STYLE('',(#12990));
#12992=SURFACE_STYLE_FILL_AREA(#12991);
#12993=SURFACE_SIDE_STYLE('',(#12992));
#12994=SURFACE_STYLE_USAGE(.BOTH.,#12993);
#12995=PRESENTATION_STYLE_ASSIGNMENT((#12994));
#12996=COLOUR_RGB('Grey',0.48,0.52,0.57);
#12997=FILL_AREA_STYLE_COLOUR('',#12996);
#12998=FILL_AREA_STYLE('',(#12997));
#12999=SURFACE_STYLE_FILL_AREA(#12998);
#13000=SURFACE_SIDE_STYLE('',(#12999));
#13001=SURFACE_STYLE_USAGE(.BOTH.,#13000);
#13002=PRESENTATION_STYLE_ASSIGNMENT((#13001));
#13003=COLOUR_RGB('Black',0.12,0.14,0.17);
#13004=FILL_AREA_STYLE_COLOUR('',#13003);
#13005=FILL_AREA_STYLE('',(#13004));
#13006=SURFACE_STYLE_FILL_AREA(#13005);
#13007=SURFACE_SIDE_STYLE('',(#13006));
#13008=SURFACE_STYLE_USAGE(.BOTH.,#13007);
#13009=PRESENTATION_STYLE_ASSIGNMENT((#13008));
#13010=COLOUR_RGB('Off White',0.89,0.88,0.83);
#13011=FILL_AREA_STYLE_COLOUR('',#13010);
#13012=FILL_AREA_STYLE('',(#13011));
#13013=SURFACE_STYLE_FILL_AREA(#13012);
#13014=SURFACE_SIDE_STYLE('',(#13013));
#13015=SURFACE_STYLE_USAGE(.BOTH.,#13014);
#13016=PRESENTATION_STYLE_ASSIGNMENT((#13015));
ENDSEC;
END-ISO-10303-21;
